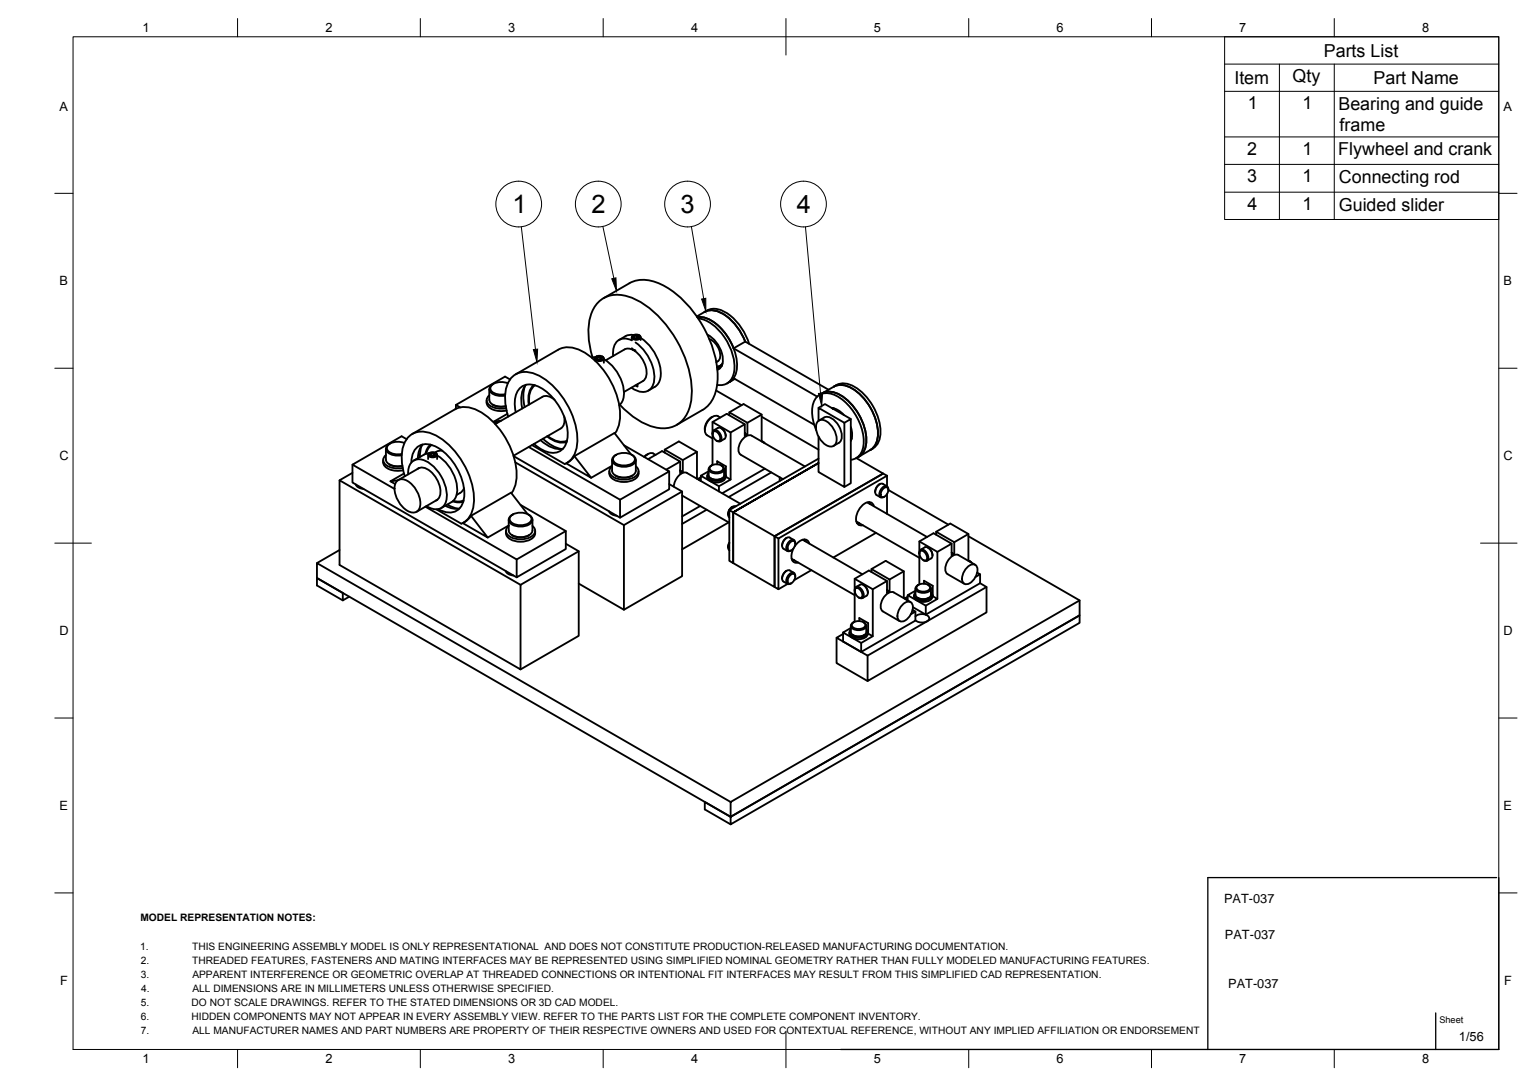
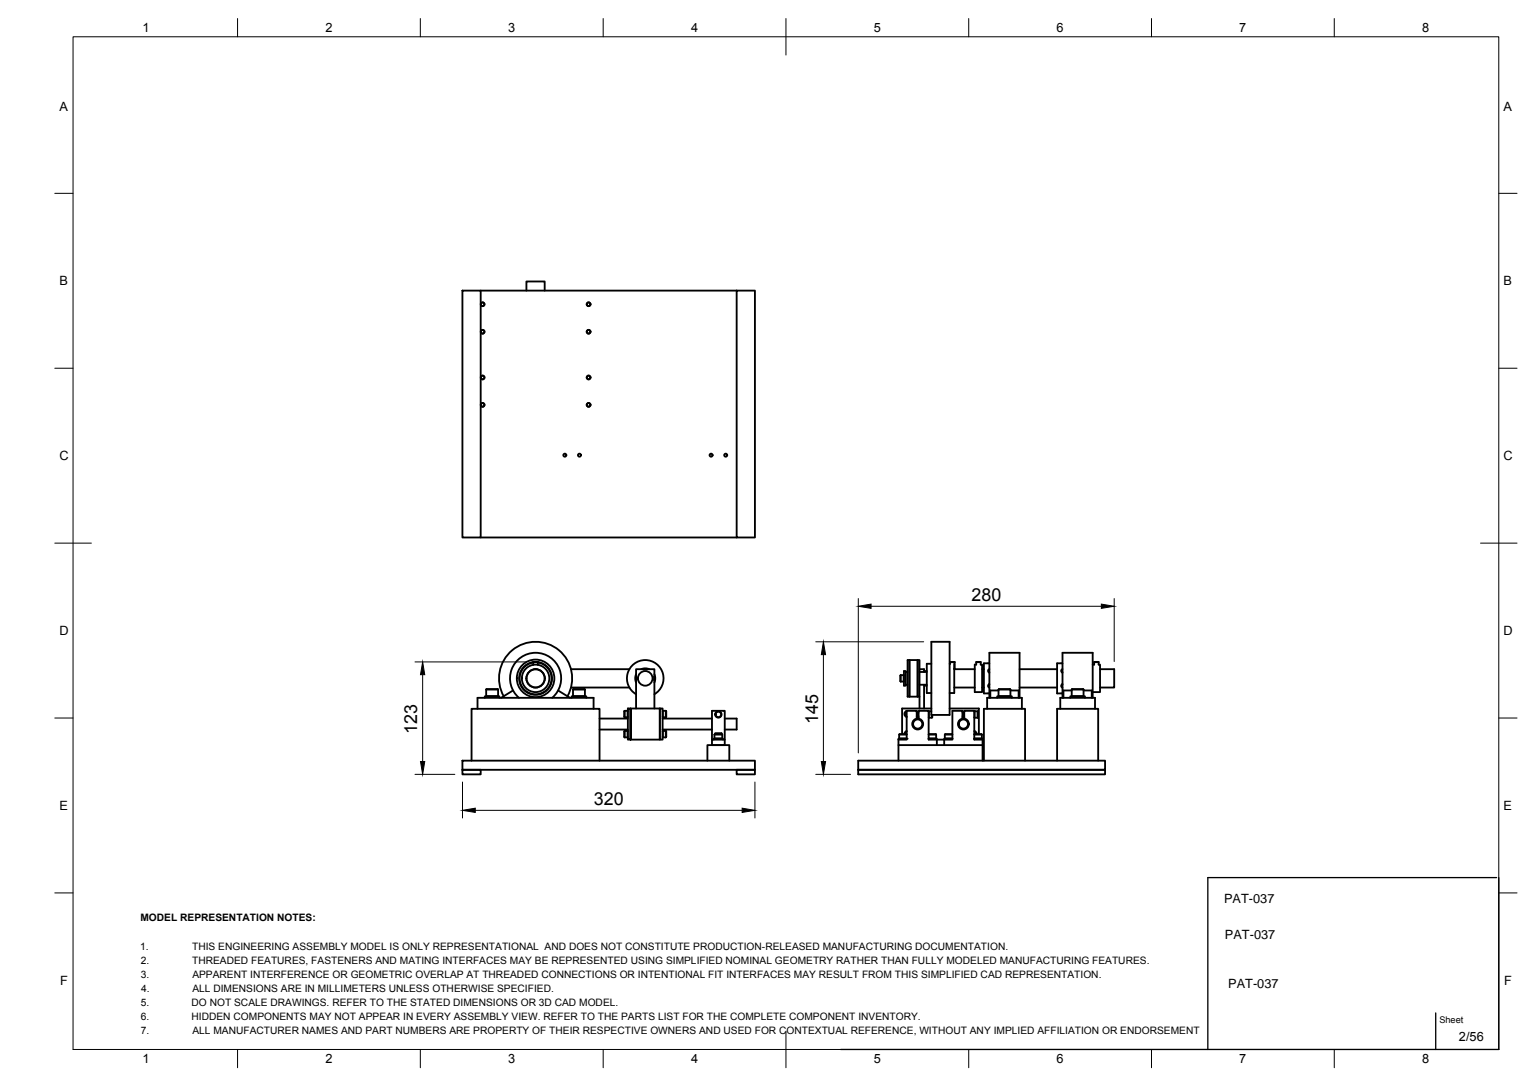
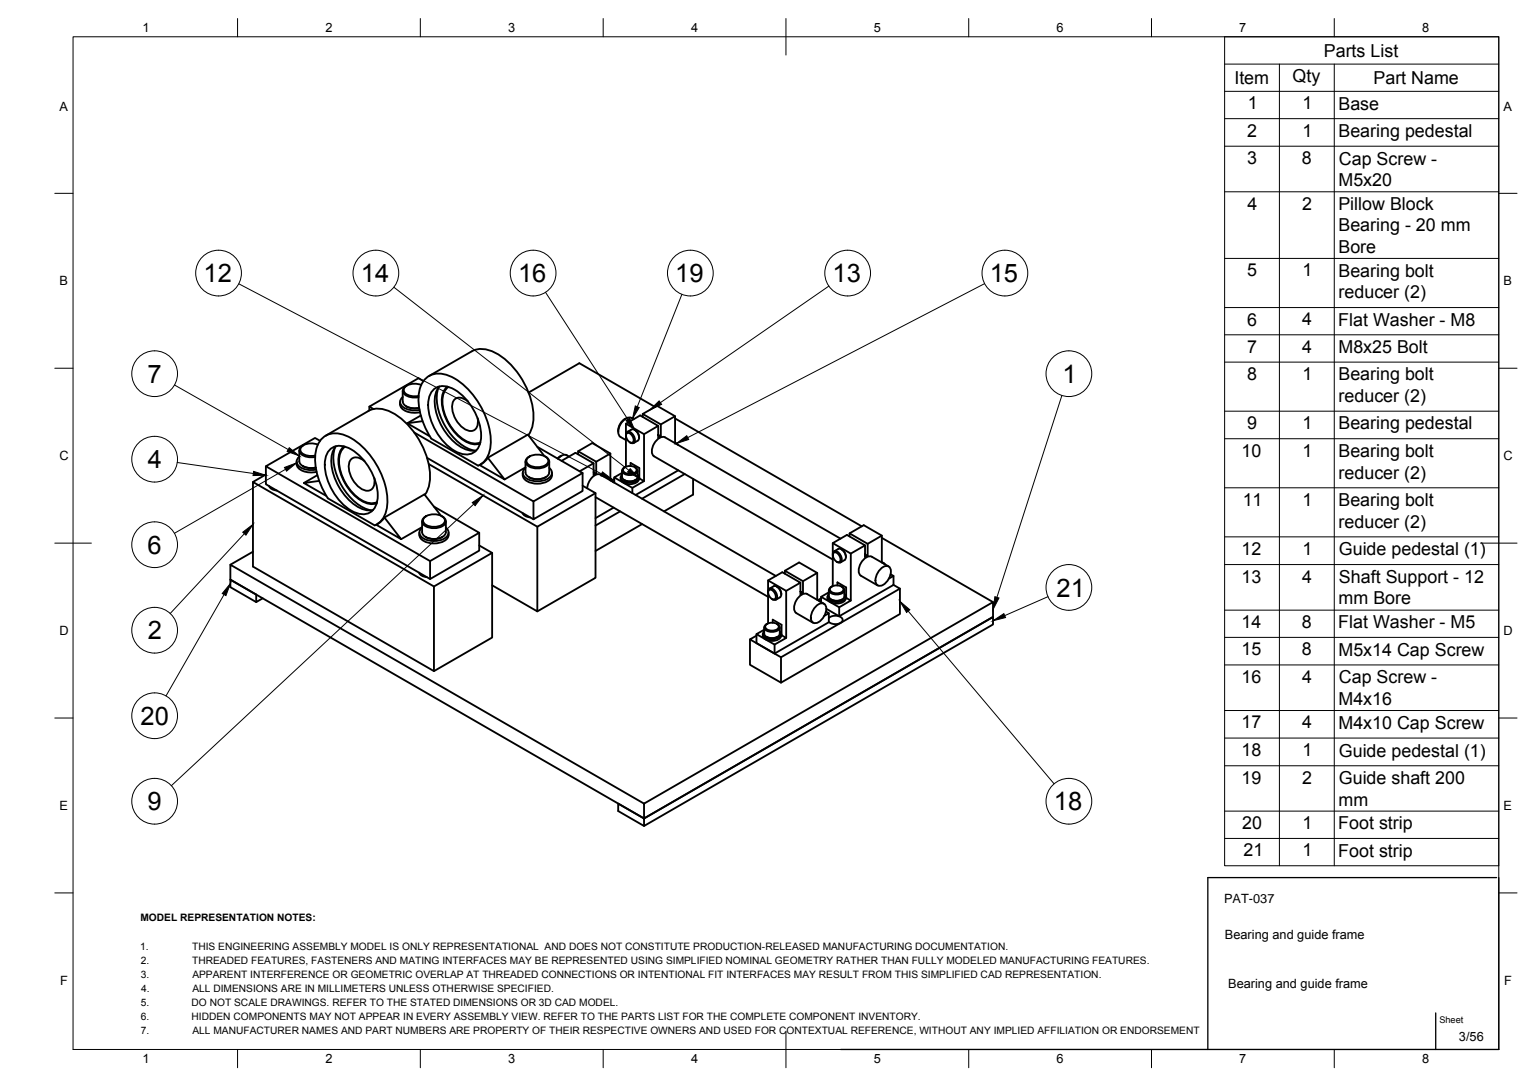
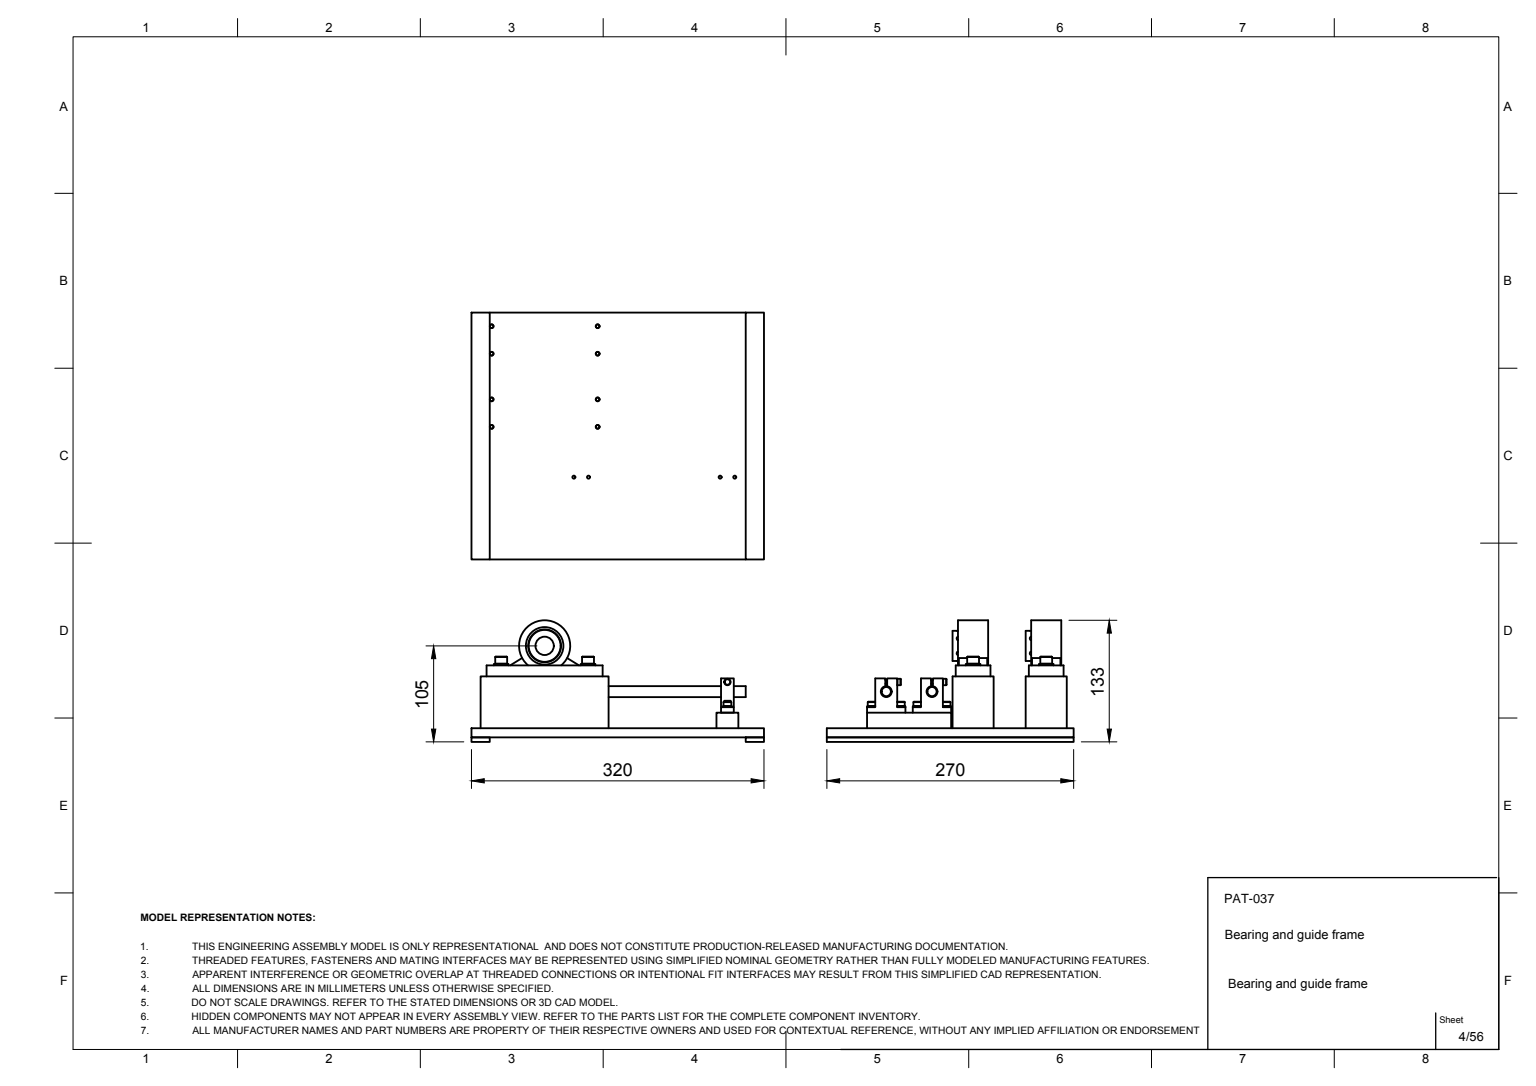
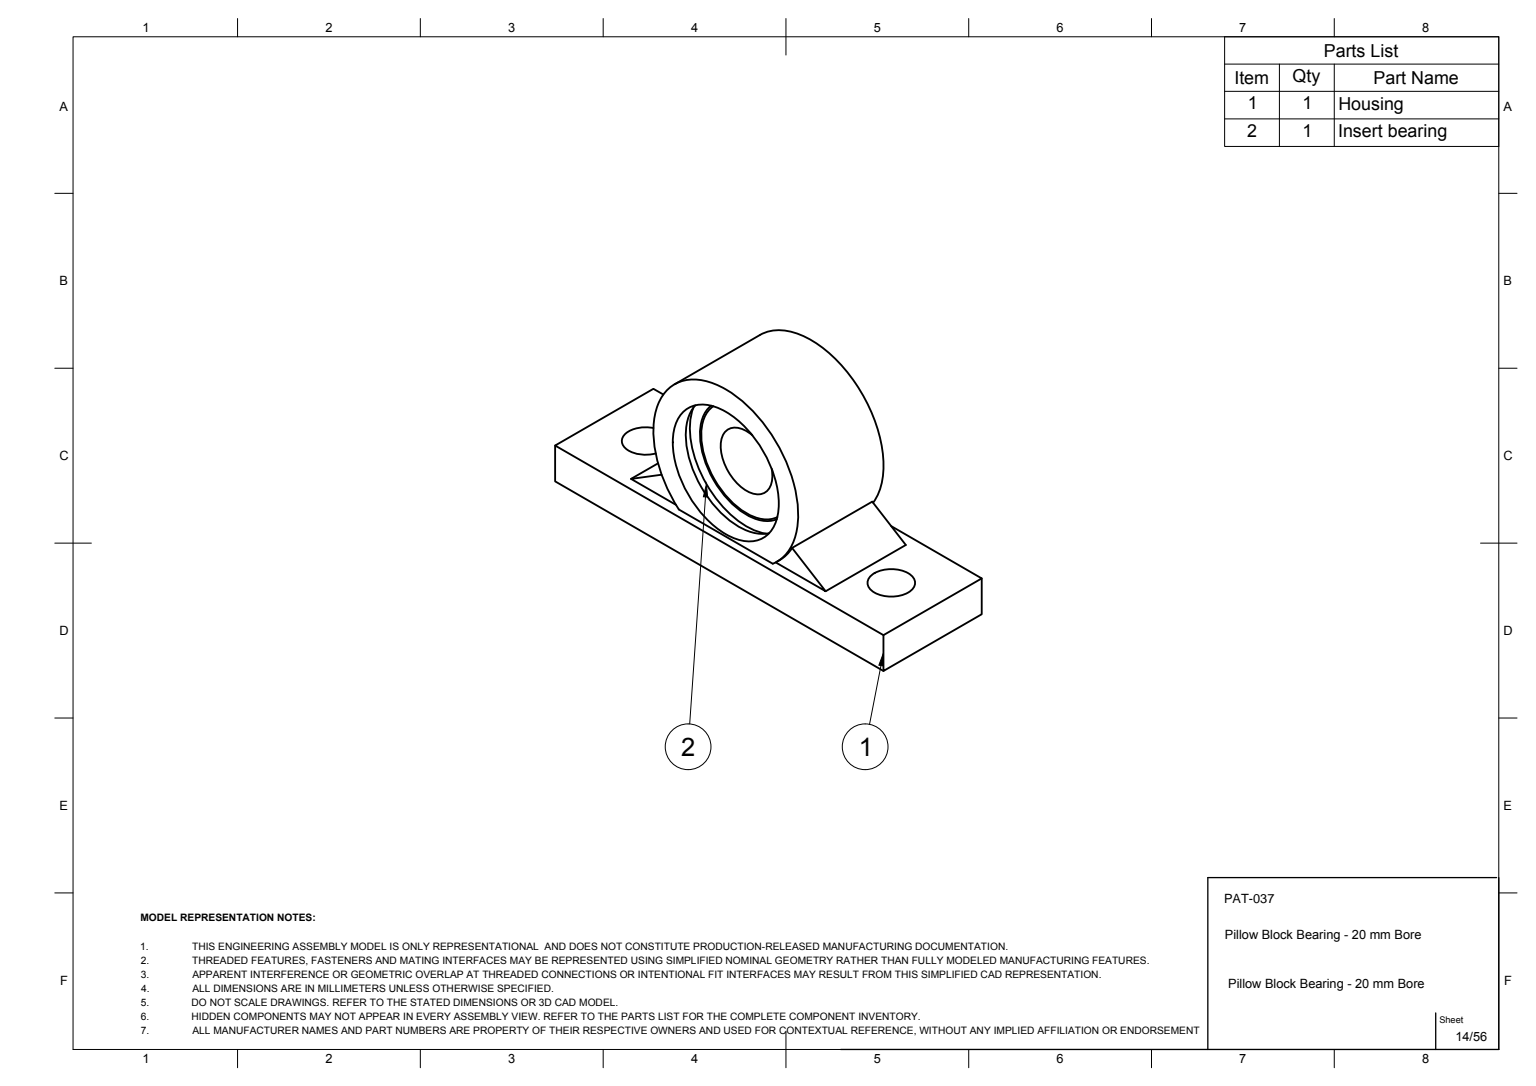
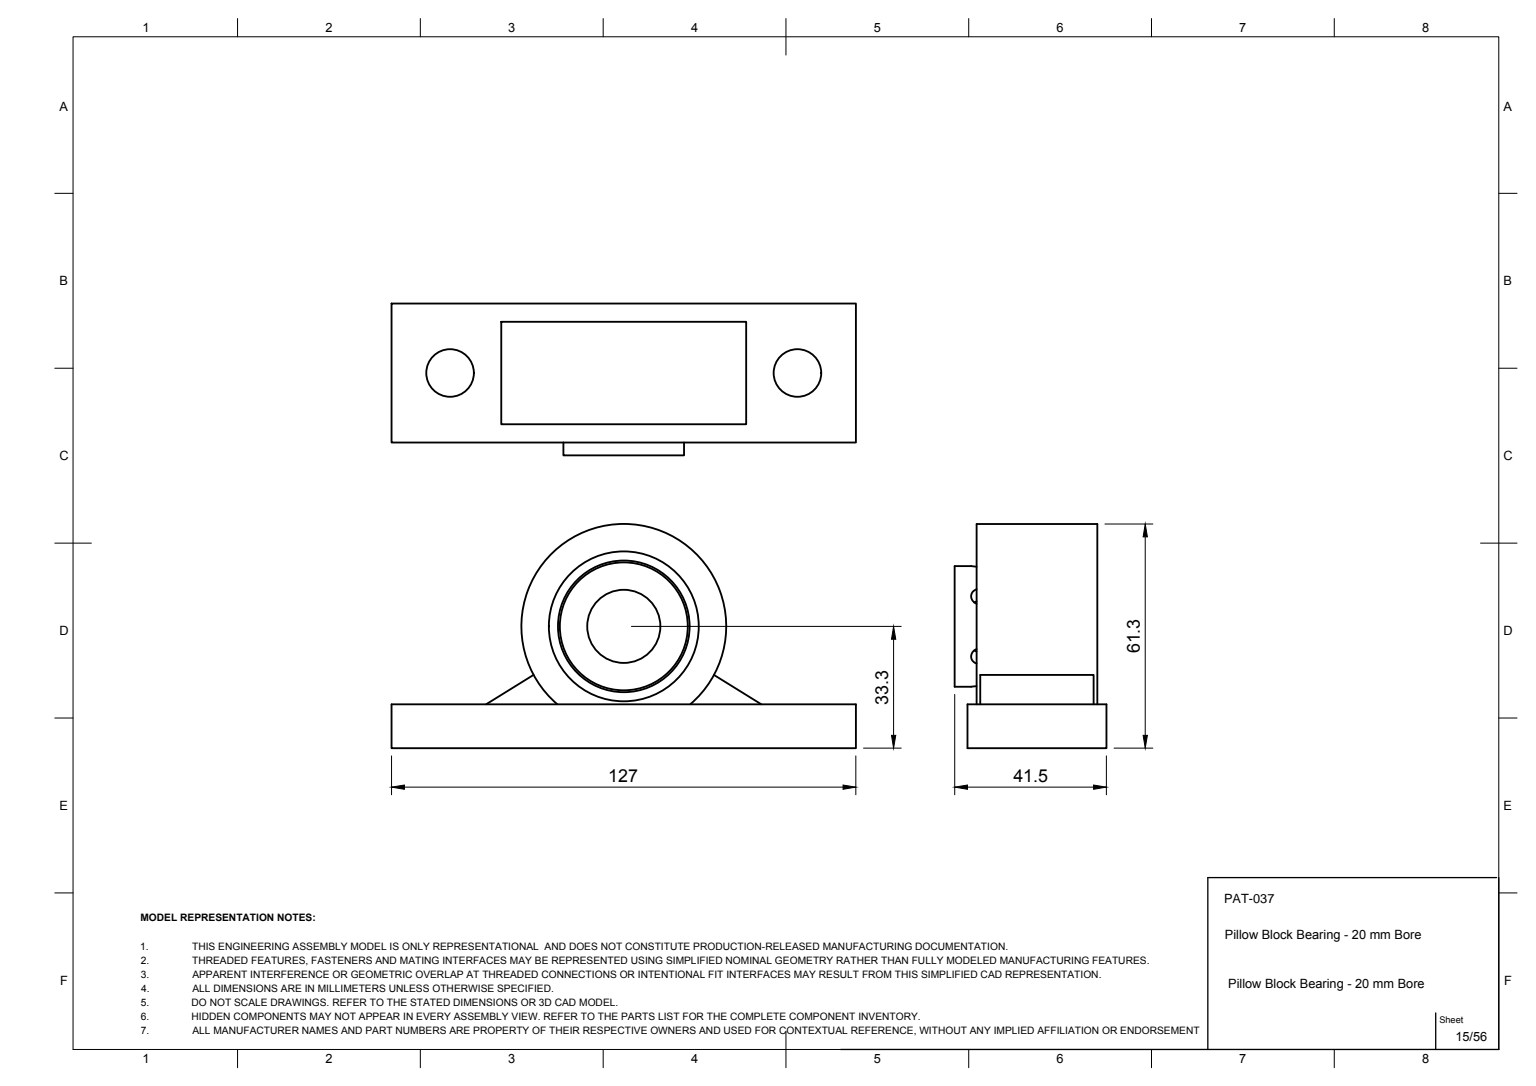
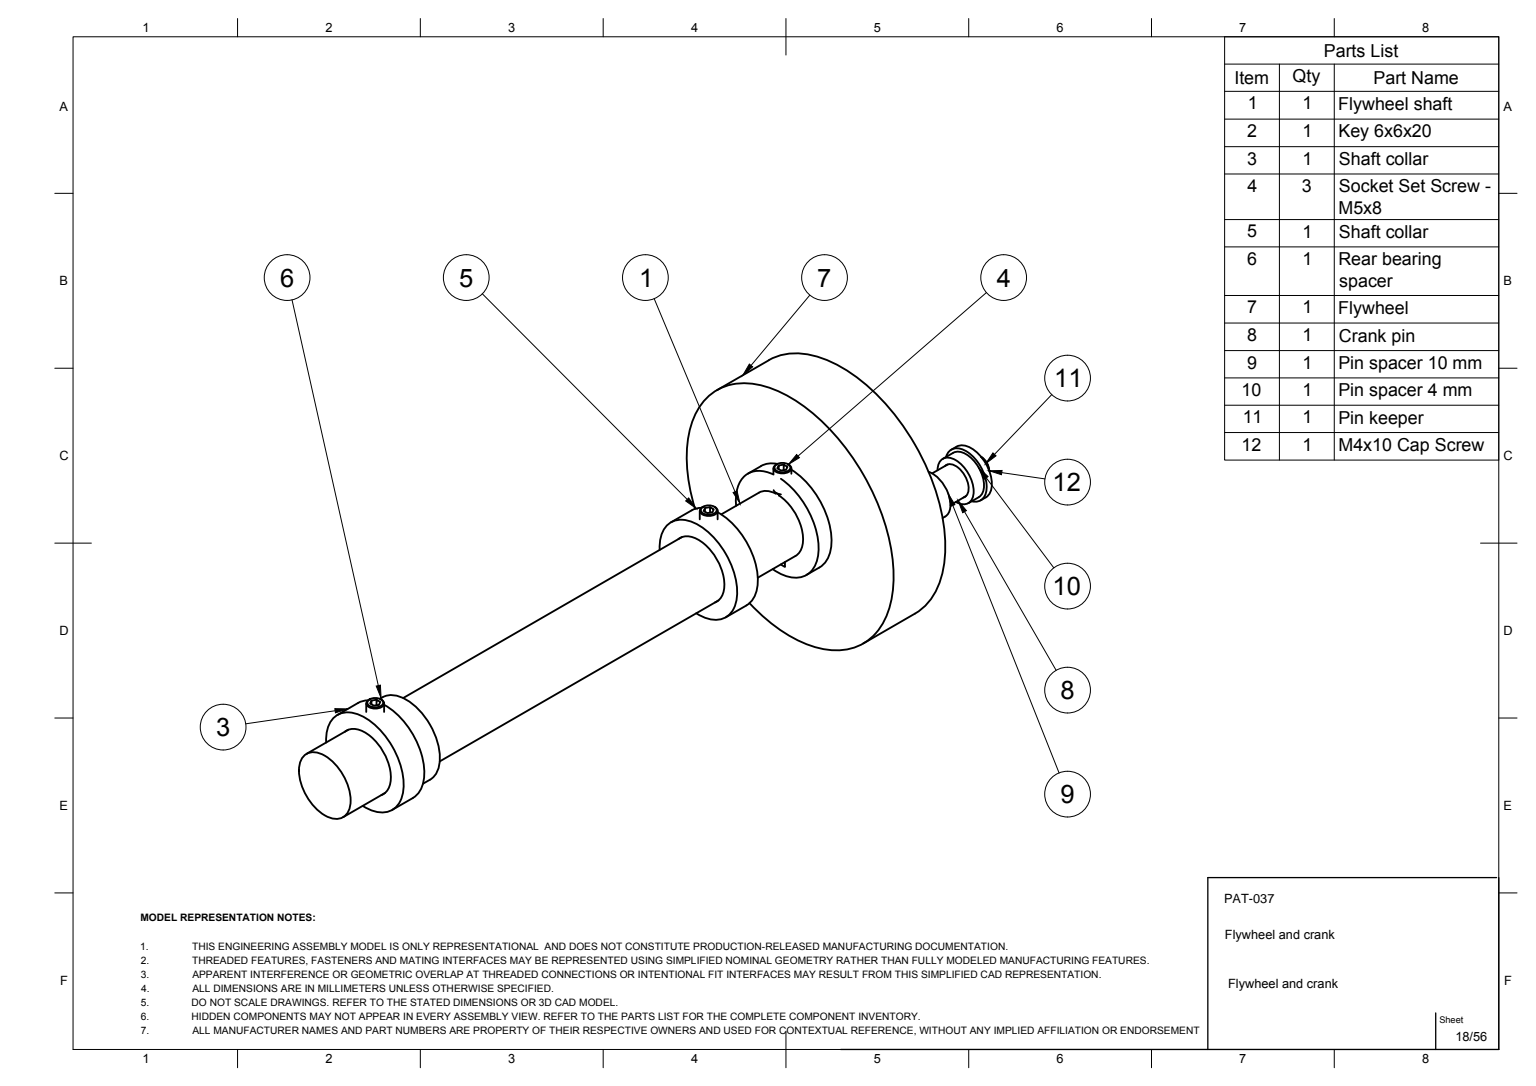
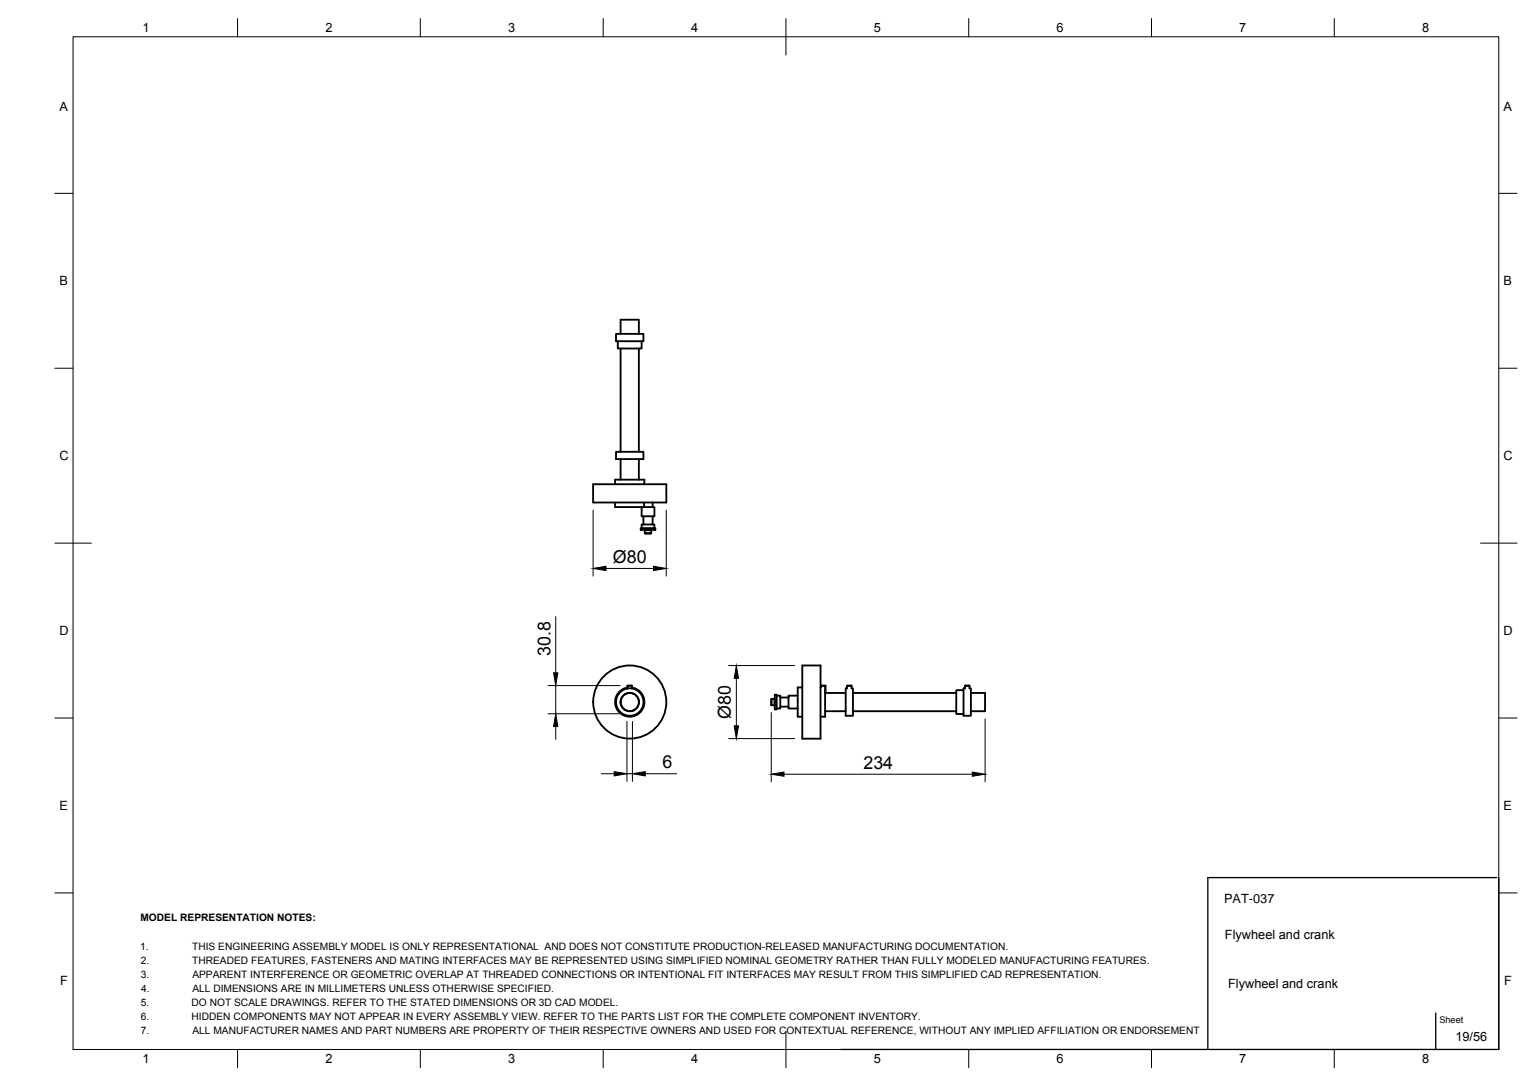
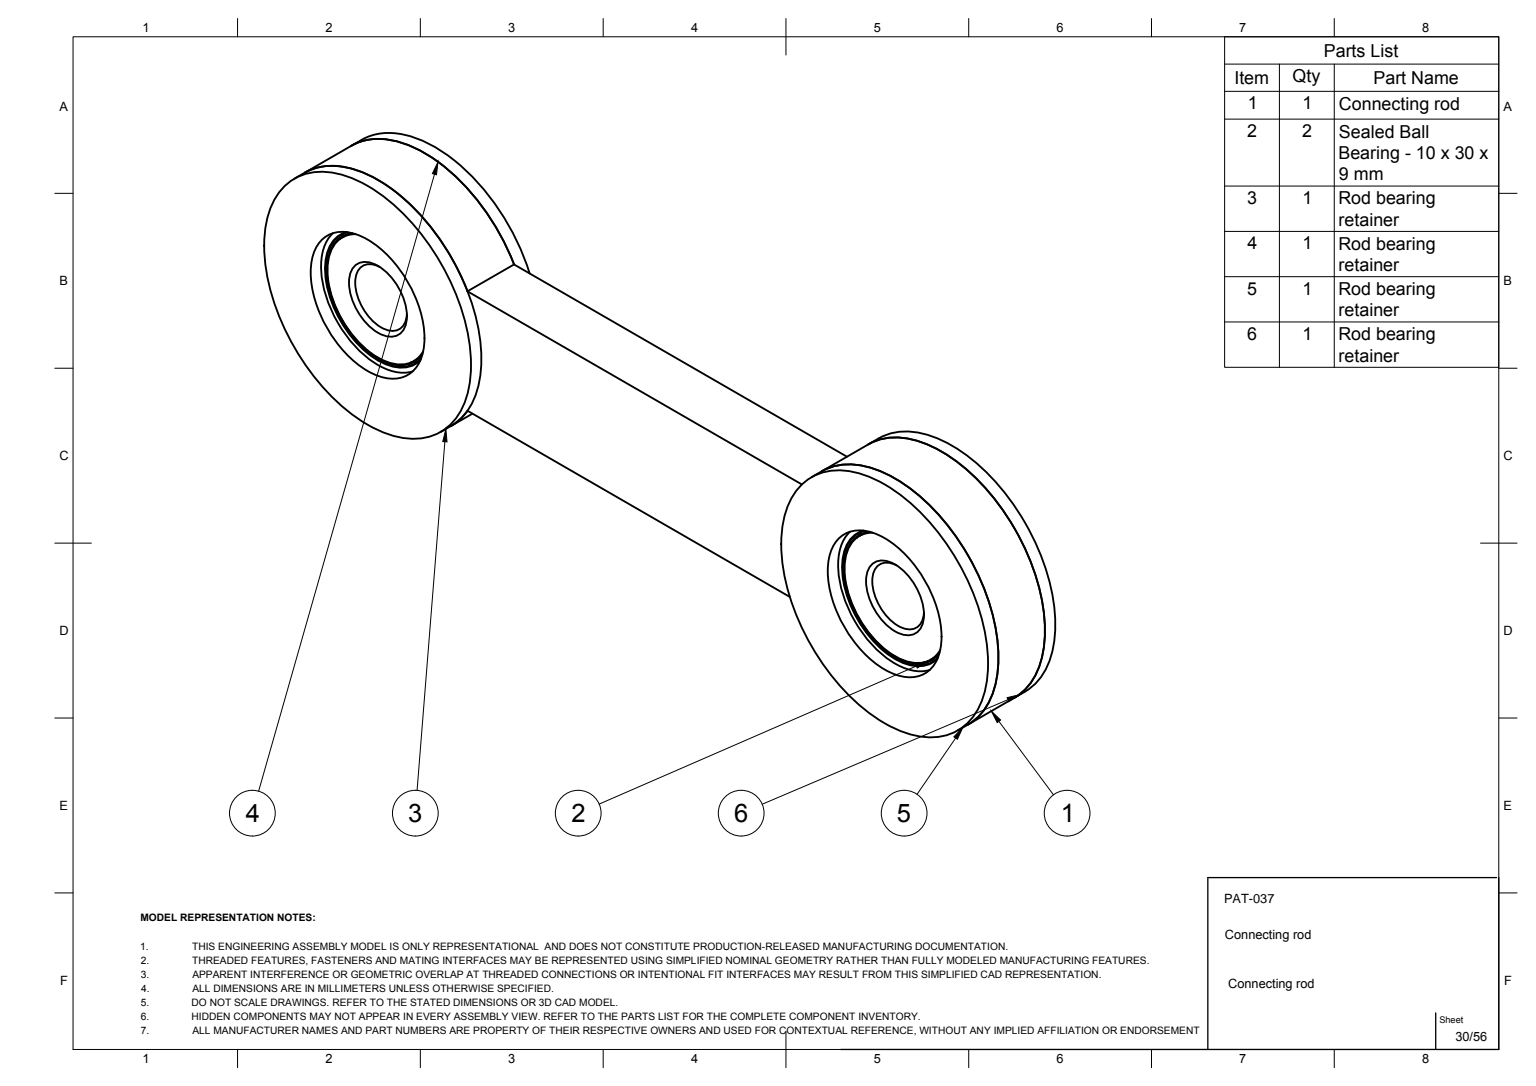
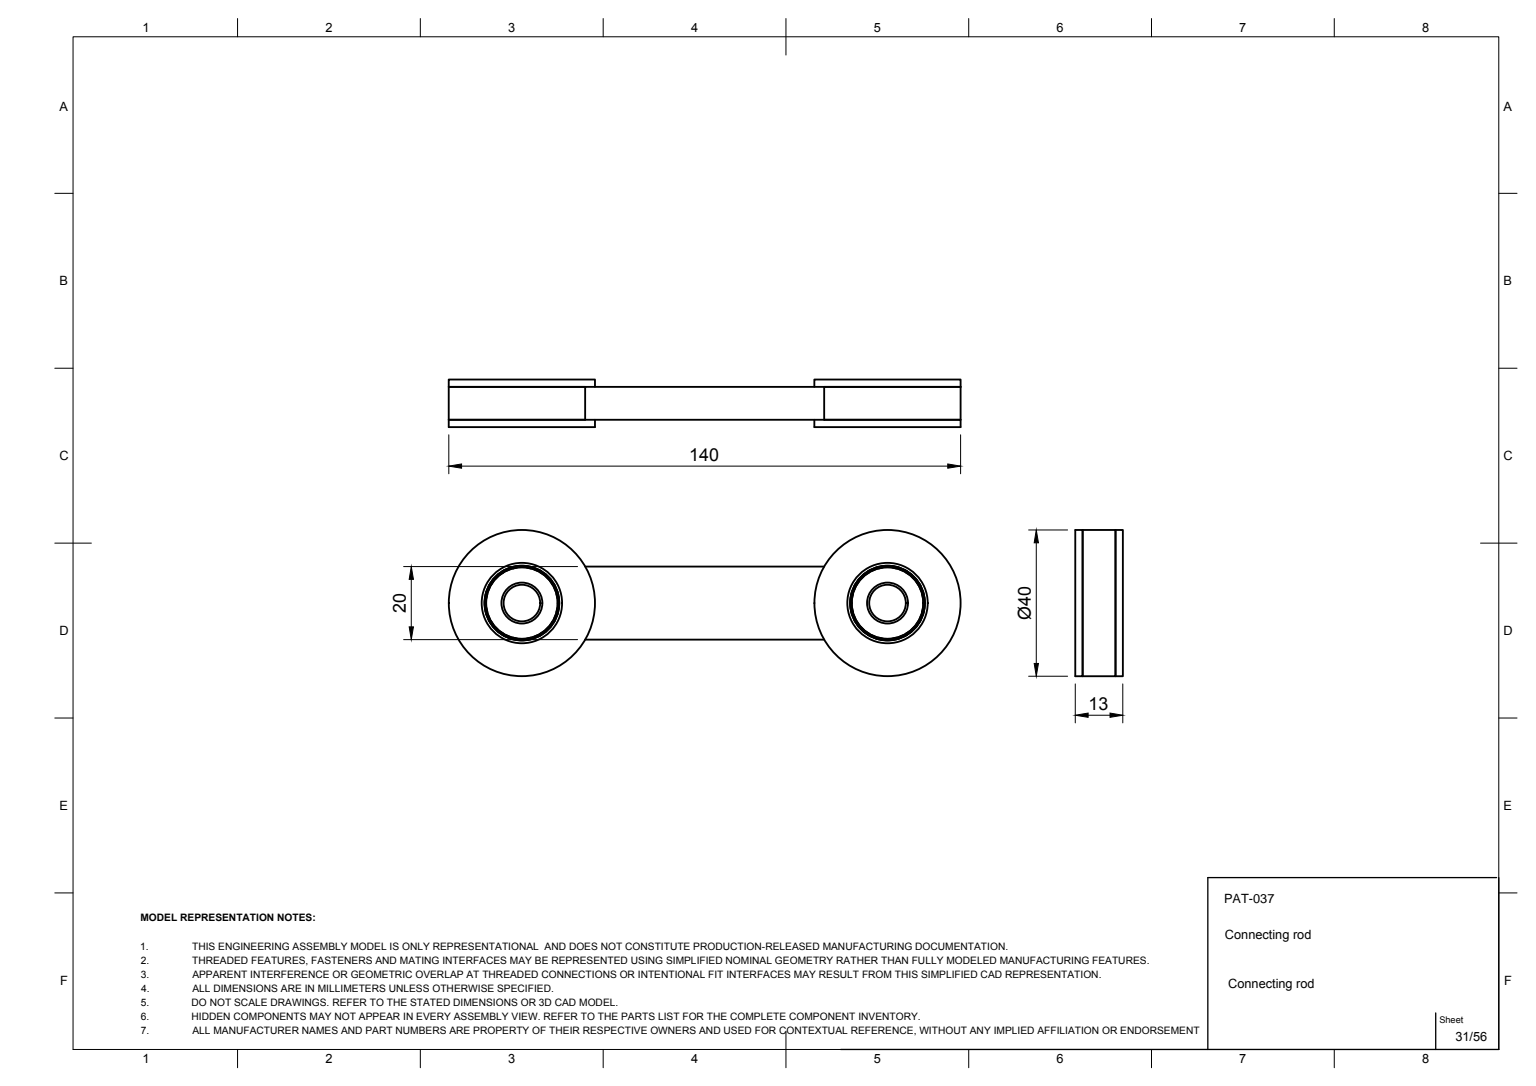
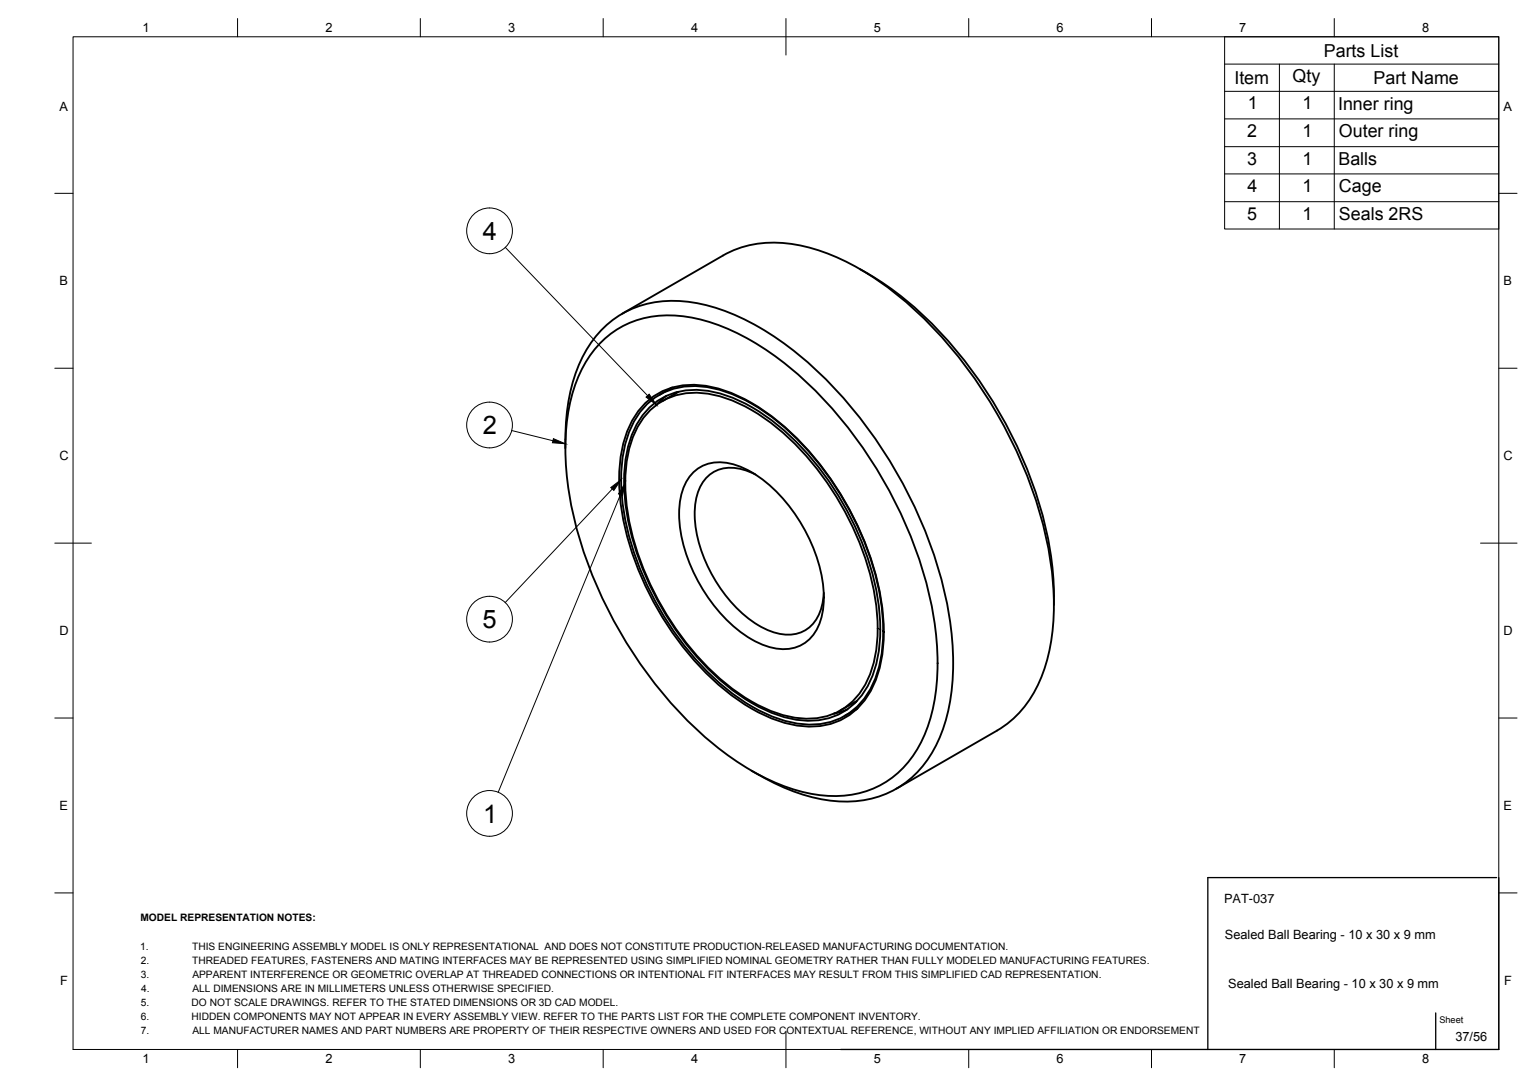
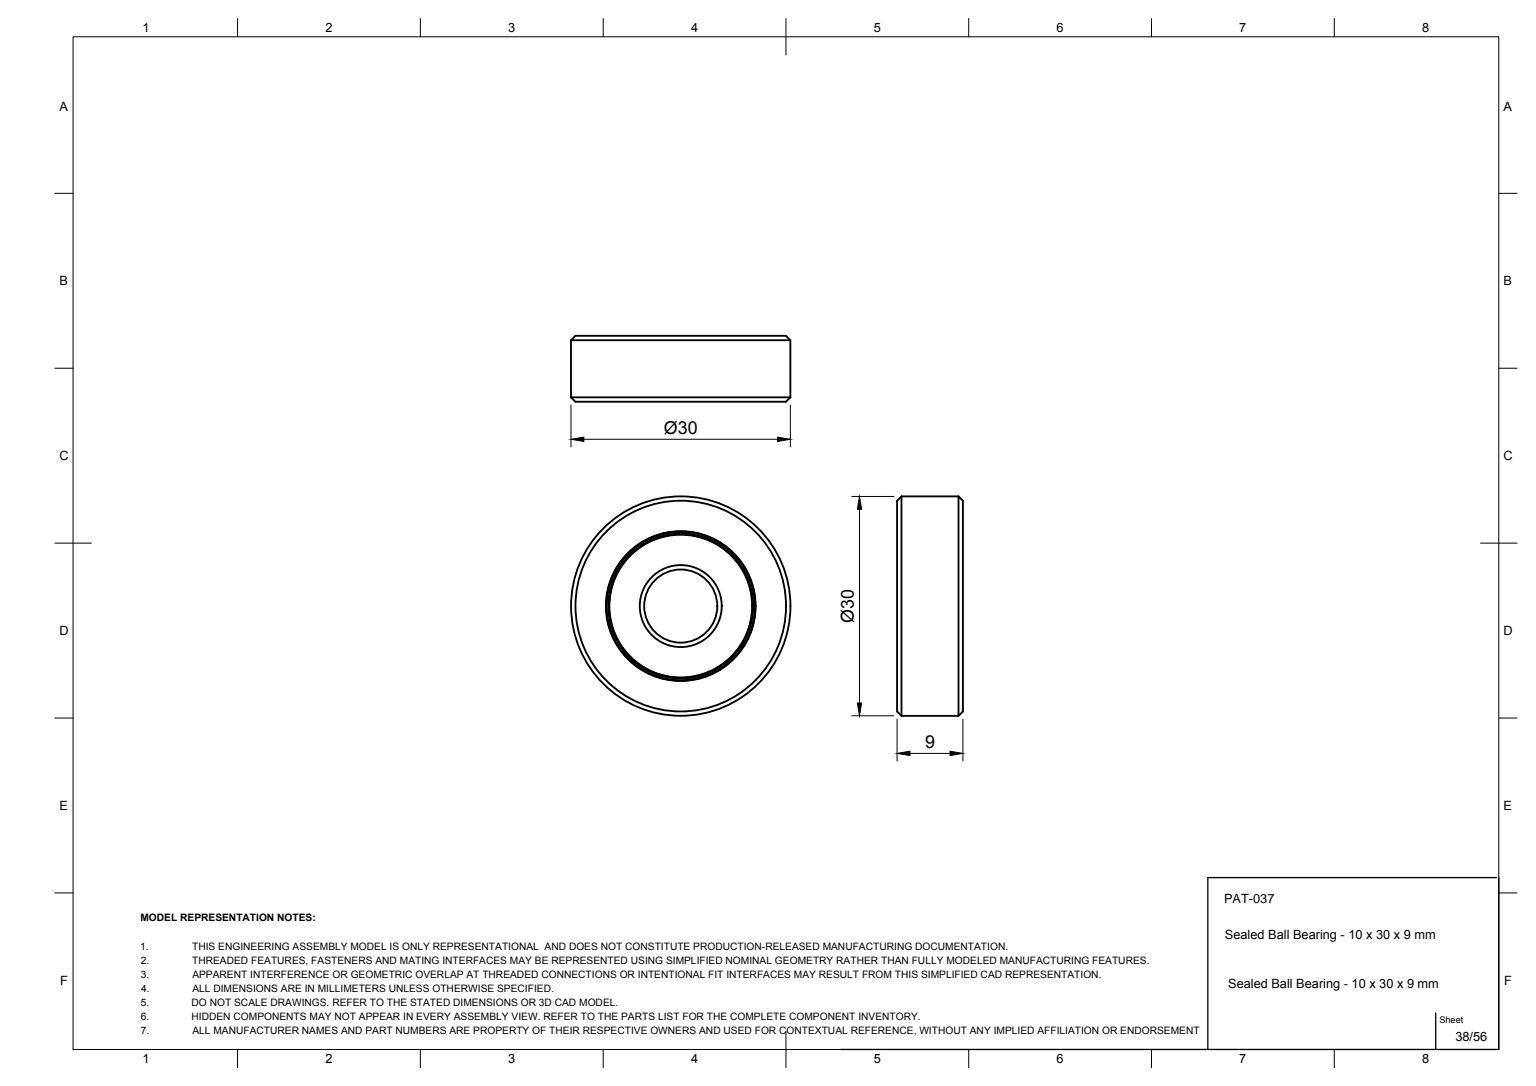
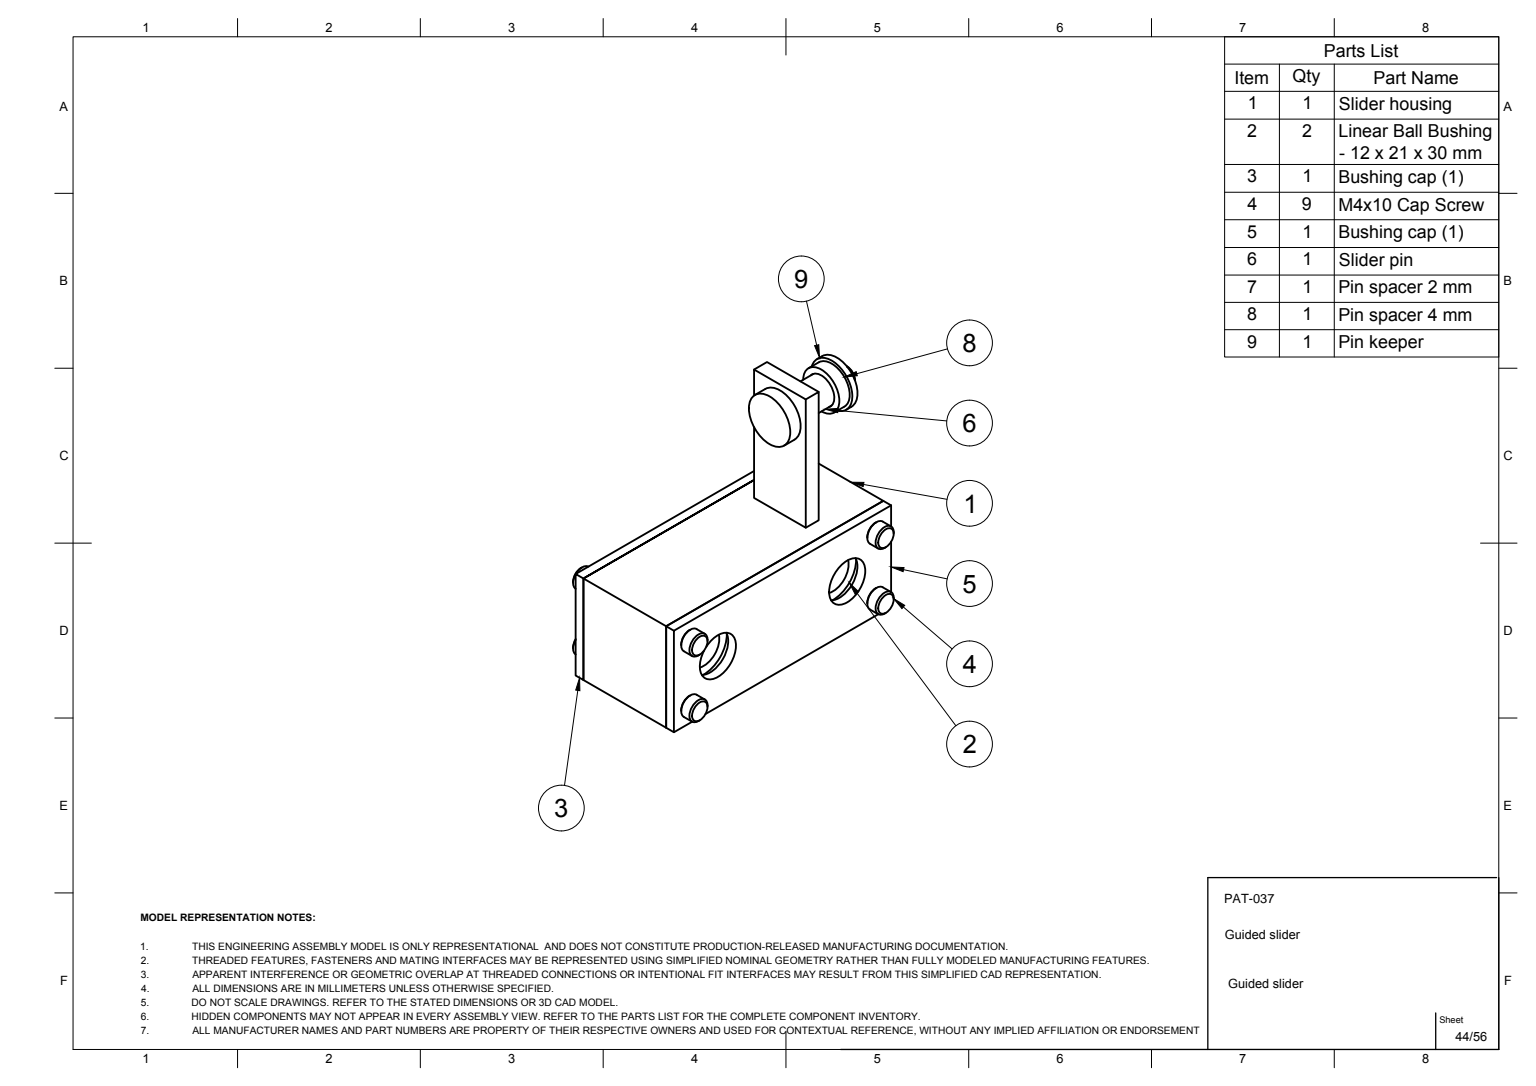
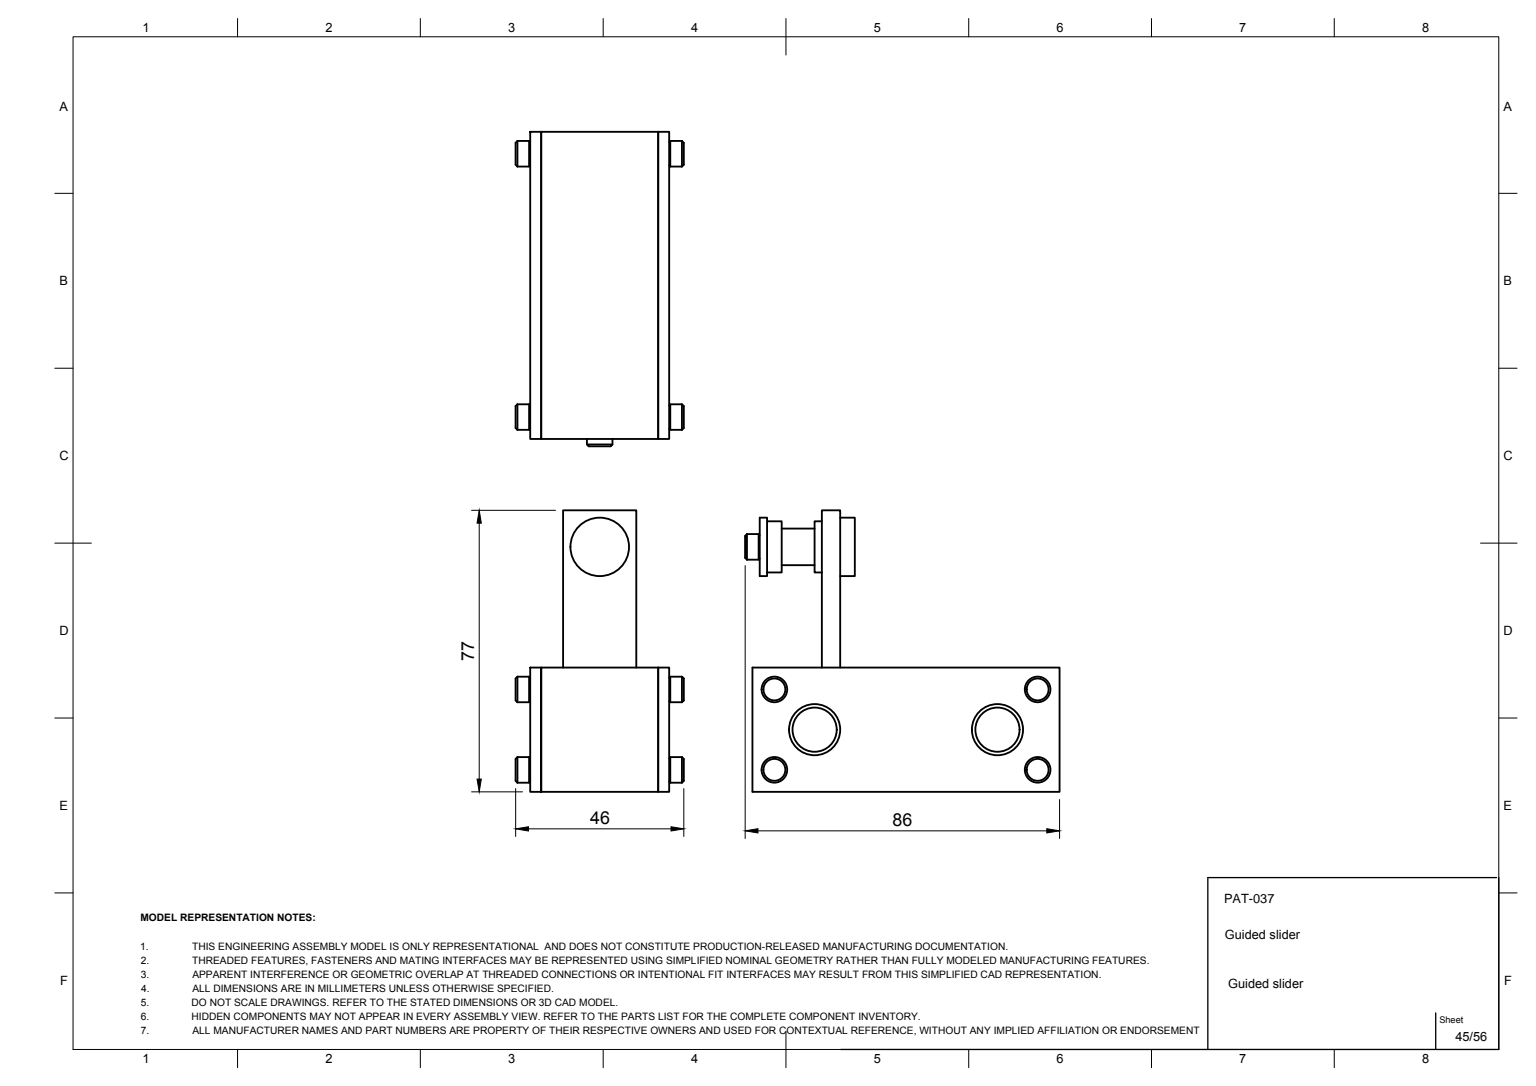
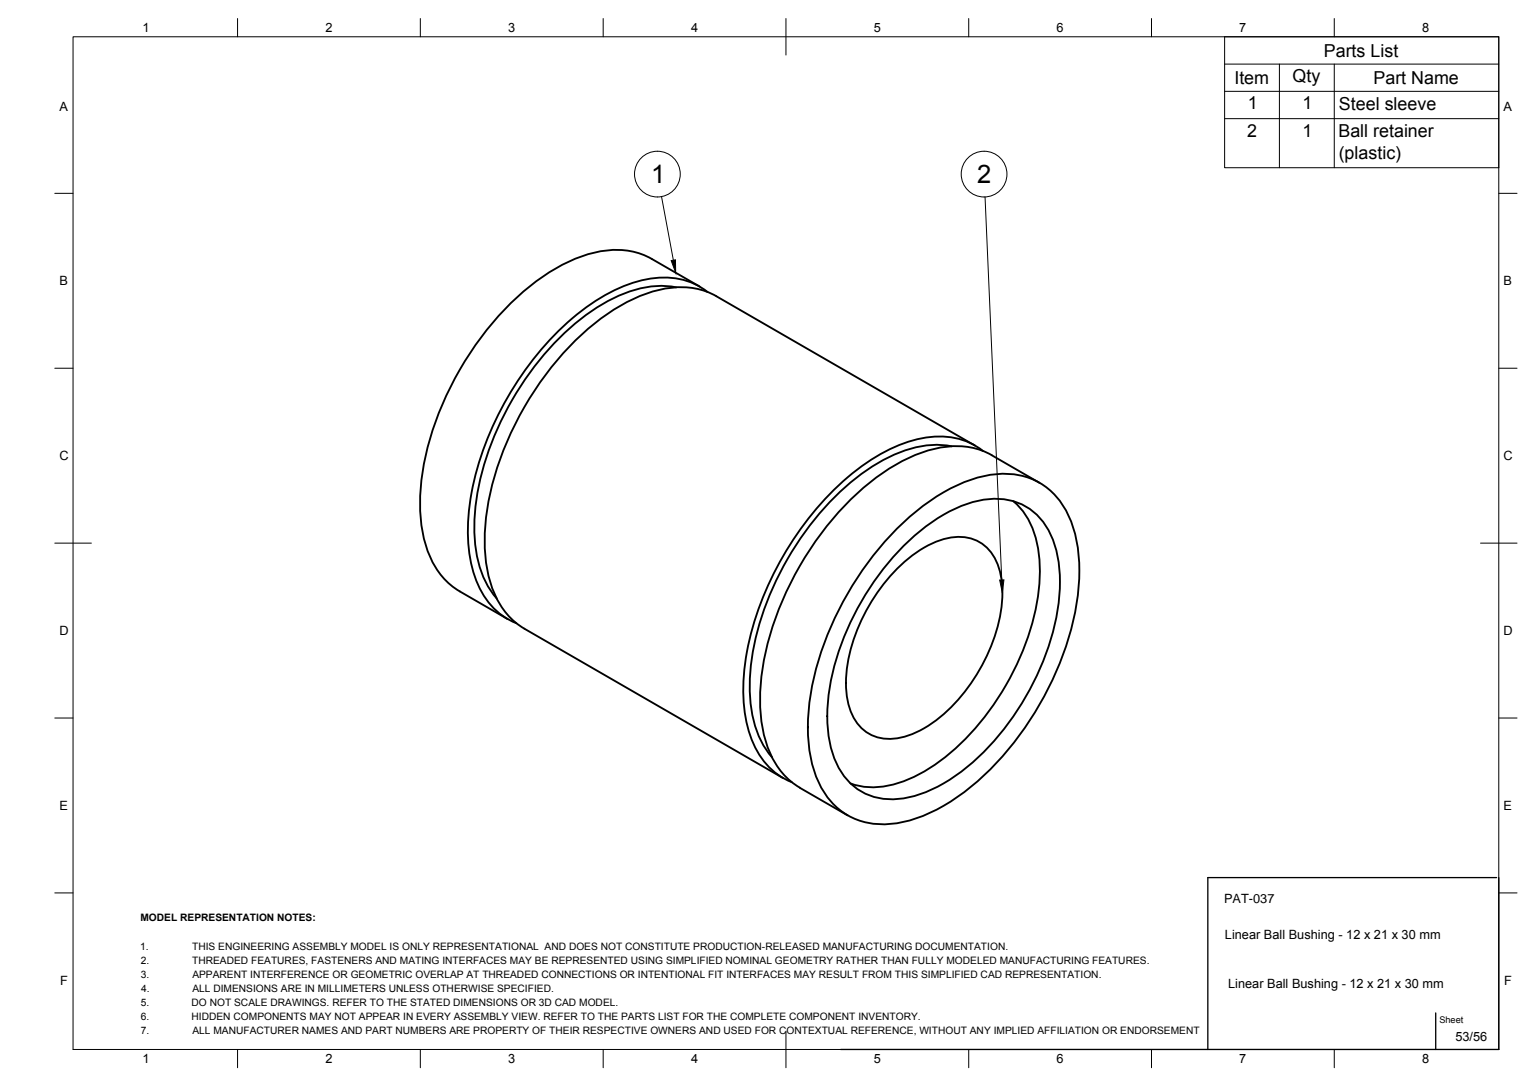
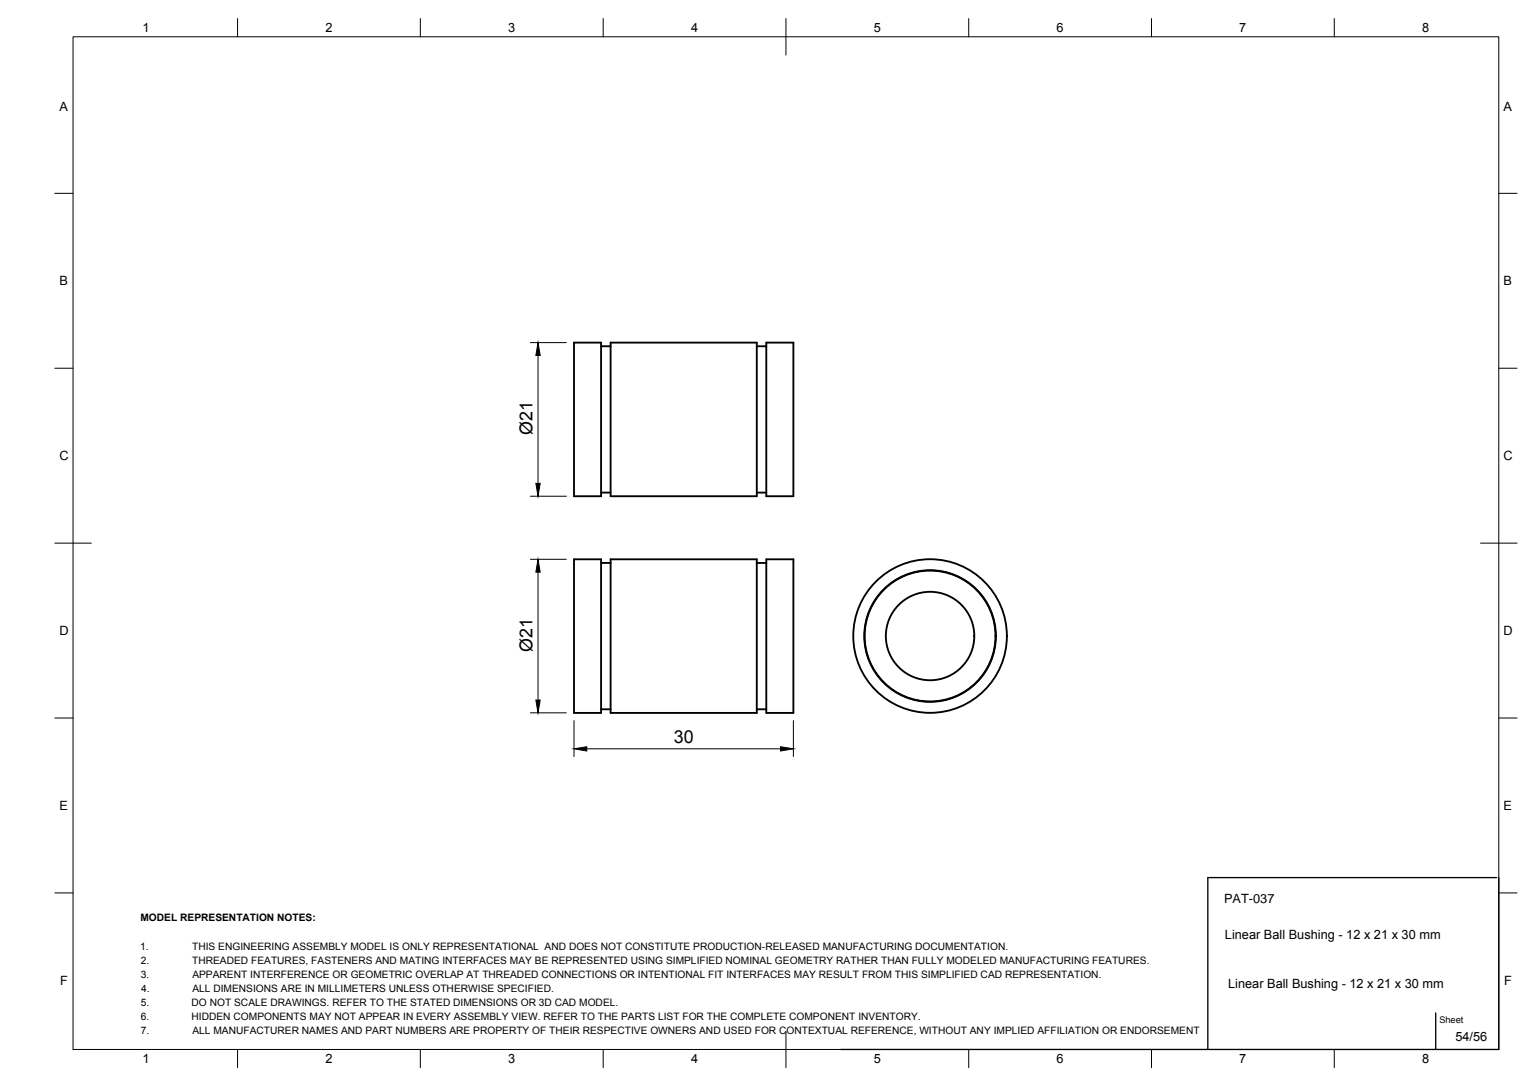
ISO-10303-21;
HEADER;
/* Generated by software containing ST-Developer
 * from STEP Tools, Inc. (www.steptools.com) 
 */

FILE_DESCRIPTION(
/* description */ ('Flywheel Crank-Slider'),
/* implementation_level */ '2;1');

FILE_NAME(
/* name */ 'PAT-037',
/* time_stamp */ '2026-10-28T03:23:13-07:00',
/* author */ (''),
/* organization */ (''),
/* preprocessor_version */ 'ST-DEVELOPER v20.2',
/* originating_system */ 'Autodesk Translation Framework v15.17.0.0',
/* authorisation */ '');

FILE_SCHEMA (('AUTOMOTIVE_DESIGN { 1 0 10303 214 3 1 1 }'));
ENDSEC;

DATA;
#10=MECHANICAL_DESIGN_GEOMETRIC_PRESENTATION_REPRESENTATION('',(#668,#669,
#670,#671,#672,#673,#674,#675,#676,#677,#678,#679,#680,#681,#682,#683,#684,
#685,#686,#687,#688,#689,#690,#691,#692,#693,#694,#695,#696,#697,#698,#699,
#700,#701,#702,#703,#704,#705,#706,#707,#708,#709,#710,#711,#712,#713,#714,
#715,#716,#717,#718,#719,#720,#721,#722,#723,#724,#725,#726,#727,#728),
#17322);
#11=TOROIDAL_SURFACE('',#10395,1.,0.247676);
#12=TOROIDAL_SURFACE('',#10415,1.,0.247676);
#13=ITEM_DEFINED_TRANSFORMATION($,$,#9973,#10042);
#14=ITEM_DEFINED_TRANSFORMATION($,$,#10014,#10043);
#15=ITEM_DEFINED_TRANSFORMATION($,$,#10394,#10522);
#16=ITEM_DEFINED_TRANSFORMATION($,$,#10414,#10523);
#17=ITEM_DEFINED_TRANSFORMATION($,$,#10434,#10524);
#18=ITEM_DEFINED_TRANSFORMATION($,$,#10451,#10525);
#19=ITEM_DEFINED_TRANSFORMATION($,$,#10505,#10526);
#20=ITEM_DEFINED_TRANSFORMATION($,$,#10340,#10527);
#21=ITEM_DEFINED_TRANSFORMATION($,$,#10357,#10528);
#22=ITEM_DEFINED_TRANSFORMATION($,$,#10366,#10529);
#23=ITEM_DEFINED_TRANSFORMATION($,$,#10375,#10530);
#24=ITEM_DEFINED_TRANSFORMATION($,$,#10384,#10531);
#25=ITEM_DEFINED_TRANSFORMATION($,$,#10393,#10532);
#26=ITEM_DEFINED_TRANSFORMATION($,$,#10393,#10533);
#27=ITEM_DEFINED_TRANSFORMATION($,$,#10660,#10709);
#28=ITEM_DEFINED_TRANSFORMATION($,$,#10692,#10710);
#29=ITEM_DEFINED_TRANSFORMATION($,$,#9687,#10735);
#30=ITEM_DEFINED_TRANSFORMATION($,$,#9730,#10736);
#31=ITEM_DEFINED_TRANSFORMATION($,$,#9773,#10737);
#32=ITEM_DEFINED_TRANSFORMATION($,$,#9782,#10738);
#33=ITEM_DEFINED_TRANSFORMATION($,$,#9791,#10739);
#34=ITEM_DEFINED_TRANSFORMATION($,$,#9834,#10740);
#35=ITEM_DEFINED_TRANSFORMATION($,$,#9843,#10741);
#36=ITEM_DEFINED_TRANSFORMATION($,$,#9852,#10742);
#37=ITEM_DEFINED_TRANSFORMATION($,$,#9892,#10743);
#38=ITEM_DEFINED_TRANSFORMATION($,$,#9932,#10744);
#39=ITEM_DEFINED_TRANSFORMATION($,$,#9939,#10745);
#40=ITEM_DEFINED_TRANSFORMATION($,$,#9946,#10746);
#41=ITEM_DEFINED_TRANSFORMATION($,$,#9946,#10747);
#42=ITEM_DEFINED_TRANSFORMATION($,$,#9946,#10748);
#43=ITEM_DEFINED_TRANSFORMATION($,$,#9946,#10749);
#44=ITEM_DEFINED_TRANSFORMATION($,$,#9972,#10750);
#45=ITEM_DEFINED_TRANSFORMATION($,$,#10044,#10751);
#46=ITEM_DEFINED_TRANSFORMATION($,$,#10053,#10752);
#47=ITEM_DEFINED_TRANSFORMATION($,$,#10044,#10753);
#48=ITEM_DEFINED_TRANSFORMATION($,$,#10053,#10754);
#49=ITEM_DEFINED_TRANSFORMATION($,$,#9946,#10755);
#50=ITEM_DEFINED_TRANSFORMATION($,$,#9946,#10756);
#51=ITEM_DEFINED_TRANSFORMATION($,$,#9946,#10757);
#52=ITEM_DEFINED_TRANSFORMATION($,$,#9946,#10758);
#53=ITEM_DEFINED_TRANSFORMATION($,$,#9972,#10759);
#54=ITEM_DEFINED_TRANSFORMATION($,$,#10044,#10760);
#55=ITEM_DEFINED_TRANSFORMATION($,$,#10053,#10761);
#56=ITEM_DEFINED_TRANSFORMATION($,$,#10044,#10762);
#57=ITEM_DEFINED_TRANSFORMATION($,$,#10053,#10763);
#58=ITEM_DEFINED_TRANSFORMATION($,$,#10077,#10764);
#59=ITEM_DEFINED_TRANSFORMATION($,$,#10115,#10765);
#60=ITEM_DEFINED_TRANSFORMATION($,$,#10126,#10766);
#61=ITEM_DEFINED_TRANSFORMATION($,$,#10115,#10767);
#62=ITEM_DEFINED_TRANSFORMATION($,$,#10126,#10768);
#63=ITEM_DEFINED_TRANSFORMATION($,$,#10150,#10769);
#64=ITEM_DEFINED_TRANSFORMATION($,$,#10077,#10770);
#65=ITEM_DEFINED_TRANSFORMATION($,$,#10115,#10771);
#66=ITEM_DEFINED_TRANSFORMATION($,$,#10126,#10772);
#67=ITEM_DEFINED_TRANSFORMATION($,$,#10115,#10773);
#68=ITEM_DEFINED_TRANSFORMATION($,$,#10126,#10774);
#69=ITEM_DEFINED_TRANSFORMATION($,$,#10150,#10775);
#70=ITEM_DEFINED_TRANSFORMATION($,$,#10711,#10776);
#71=ITEM_DEFINED_TRANSFORMATION($,$,#10711,#10777);
#72=ITEM_DEFINED_TRANSFORMATION($,$,#10077,#10778);
#73=ITEM_DEFINED_TRANSFORMATION($,$,#10115,#10779);
#74=ITEM_DEFINED_TRANSFORMATION($,$,#10126,#10780);
#75=ITEM_DEFINED_TRANSFORMATION($,$,#10115,#10781);
#76=ITEM_DEFINED_TRANSFORMATION($,$,#10126,#10782);
#77=ITEM_DEFINED_TRANSFORMATION($,$,#10150,#10783);
#78=ITEM_DEFINED_TRANSFORMATION($,$,#10077,#10784);
#79=ITEM_DEFINED_TRANSFORMATION($,$,#10115,#10785);
#80=ITEM_DEFINED_TRANSFORMATION($,$,#10126,#10786);
#81=ITEM_DEFINED_TRANSFORMATION($,$,#10115,#10787);
#82=ITEM_DEFINED_TRANSFORMATION($,$,#10126,#10788);
#83=ITEM_DEFINED_TRANSFORMATION($,$,#10150,#10789);
#84=ITEM_DEFINED_TRANSFORMATION($,$,#10711,#10790);
#85=ITEM_DEFINED_TRANSFORMATION($,$,#10711,#10791);
#86=ITEM_DEFINED_TRANSFORMATION($,$,#10176,#10792);
#87=ITEM_DEFINED_TRANSFORMATION($,$,#10176,#10793);
#88=ITEM_DEFINED_TRANSFORMATION($,$,#10185,#10794);
#89=ITEM_DEFINED_TRANSFORMATION($,$,#10197,#10795);
#90=ITEM_DEFINED_TRANSFORMATION($,$,#10212,#10796);
#91=ITEM_DEFINED_TRANSFORMATION($,$,#10227,#10797);
#92=ITEM_DEFINED_TRANSFORMATION($,$,#10236,#10798);
#93=ITEM_DEFINED_TRANSFORMATION($,$,#10270,#10799);
#94=ITEM_DEFINED_TRANSFORMATION($,$,#10284,#10800);
#95=ITEM_DEFINED_TRANSFORMATION($,$,#10293,#10801);
#96=ITEM_DEFINED_TRANSFORMATION($,$,#10302,#10802);
#97=ITEM_DEFINED_TRANSFORMATION($,$,#10311,#10803);
#98=ITEM_DEFINED_TRANSFORMATION($,$,#10322,#10804);
#99=ITEM_DEFINED_TRANSFORMATION($,$,#10322,#10805);
#100=ITEM_DEFINED_TRANSFORMATION($,$,#10322,#10806);
#101=ITEM_DEFINED_TRANSFORMATION($,$,#10711,#10807);
#102=ITEM_DEFINED_TRANSFORMATION($,$,#10535,#10808);
#103=ITEM_DEFINED_TRANSFORMATION($,$,#10568,#10809);
#104=ITEM_DEFINED_TRANSFORMATION($,$,#10593,#10810);
#105=ITEM_DEFINED_TRANSFORMATION($,$,#10618,#10811);
#106=ITEM_DEFINED_TRANSFORMATION($,$,#10632,#10812);
#107=ITEM_DEFINED_TRANSFORMATION($,$,#10641,#10813);
#108=ITEM_DEFINED_TRANSFORMATION($,$,#10650,#10814);
#109=ITEM_DEFINED_TRANSFORMATION($,$,#10659,#10815);
#110=ITEM_DEFINED_TRANSFORMATION($,$,#10659,#10816);
#111=ITEM_DEFINED_TRANSFORMATION($,$,#10711,#10817);
#112=ITEM_DEFINED_TRANSFORMATION($,$,#10711,#10818);
#113=ITEM_DEFINED_TRANSFORMATION($,$,#10711,#10819);
#114=ITEM_DEFINED_TRANSFORMATION($,$,#10711,#10820);
#115=ITEM_DEFINED_TRANSFORMATION($,$,#10711,#10821);
#116=ITEM_DEFINED_TRANSFORMATION($,$,#10711,#10822);
#117=ITEM_DEFINED_TRANSFORMATION($,$,#10711,#10823);
#118=ITEM_DEFINED_TRANSFORMATION($,$,#10711,#10824);
#119=ITEM_DEFINED_TRANSFORMATION($,$,#10711,#10825);
#120=ITEM_DEFINED_TRANSFORMATION($,$,#9686,#10826);
#121=ITEM_DEFINED_TRANSFORMATION($,$,#10184,#10827);
#122=ITEM_DEFINED_TRANSFORMATION($,$,#10339,#10828);
#123=ITEM_DEFINED_TRANSFORMATION($,$,#10534,#10829);
#124=(
REPRESENTATION_RELATIONSHIP($,$,#17573,#17572)
REPRESENTATION_RELATIONSHIP_WITH_TRANSFORMATION(#13)
SHAPE_REPRESENTATION_RELATIONSHIP()
);
#125=(
REPRESENTATION_RELATIONSHIP($,$,#17574,#17572)
REPRESENTATION_RELATIONSHIP_WITH_TRANSFORMATION(#14)
SHAPE_REPRESENTATION_RELATIONSHIP()
);
#126=(
REPRESENTATION_RELATIONSHIP($,$,#17601,#17600)
REPRESENTATION_RELATIONSHIP_WITH_TRANSFORMATION(#15)
SHAPE_REPRESENTATION_RELATIONSHIP()
);
#127=(
REPRESENTATION_RELATIONSHIP($,$,#17602,#17600)
REPRESENTATION_RELATIONSHIP_WITH_TRANSFORMATION(#16)
SHAPE_REPRESENTATION_RELATIONSHIP()
);
#128=(
REPRESENTATION_RELATIONSHIP($,$,#17603,#17600)
REPRESENTATION_RELATIONSHIP_WITH_TRANSFORMATION(#17)
SHAPE_REPRESENTATION_RELATIONSHIP()
);
#129=(
REPRESENTATION_RELATIONSHIP($,$,#17604,#17600)
REPRESENTATION_RELATIONSHIP_WITH_TRANSFORMATION(#18)
SHAPE_REPRESENTATION_RELATIONSHIP()
);
#130=(
REPRESENTATION_RELATIONSHIP($,$,#17605,#17600)
REPRESENTATION_RELATIONSHIP_WITH_TRANSFORMATION(#19)
SHAPE_REPRESENTATION_RELATIONSHIP()
);
#131=(
REPRESENTATION_RELATIONSHIP($,$,#17595,#17594)
REPRESENTATION_RELATIONSHIP_WITH_TRANSFORMATION(#20)
SHAPE_REPRESENTATION_RELATIONSHIP()
);
#132=(
REPRESENTATION_RELATIONSHIP($,$,#17596,#17594)
REPRESENTATION_RELATIONSHIP_WITH_TRANSFORMATION(#21)
SHAPE_REPRESENTATION_RELATIONSHIP()
);
#133=(
REPRESENTATION_RELATIONSHIP($,$,#17597,#17594)
REPRESENTATION_RELATIONSHIP_WITH_TRANSFORMATION(#22)
SHAPE_REPRESENTATION_RELATIONSHIP()
);
#134=(
REPRESENTATION_RELATIONSHIP($,$,#17598,#17594)
REPRESENTATION_RELATIONSHIP_WITH_TRANSFORMATION(#23)
SHAPE_REPRESENTATION_RELATIONSHIP()
);
#135=(
REPRESENTATION_RELATIONSHIP($,$,#17599,#17594)
REPRESENTATION_RELATIONSHIP_WITH_TRANSFORMATION(#24)
SHAPE_REPRESENTATION_RELATIONSHIP()
);
#136=(
REPRESENTATION_RELATIONSHIP($,$,#17600,#17594)
REPRESENTATION_RELATIONSHIP_WITH_TRANSFORMATION(#25)
SHAPE_REPRESENTATION_RELATIONSHIP()
);
#137=(
REPRESENTATION_RELATIONSHIP($,$,#17600,#17594)
REPRESENTATION_RELATIONSHIP_WITH_TRANSFORMATION(#26)
SHAPE_REPRESENTATION_RELATIONSHIP()
);
#138=(
REPRESENTATION_RELATIONSHIP($,$,#17615,#17614)
REPRESENTATION_RELATIONSHIP_WITH_TRANSFORMATION(#27)
SHAPE_REPRESENTATION_RELATIONSHIP()
);
#139=(
REPRESENTATION_RELATIONSHIP($,$,#17616,#17614)
REPRESENTATION_RELATIONSHIP_WITH_TRANSFORMATION(#28)
SHAPE_REPRESENTATION_RELATIONSHIP()
);
#140=(
REPRESENTATION_RELATIONSHIP($,$,#17560,#17559)
REPRESENTATION_RELATIONSHIP_WITH_TRANSFORMATION(#29)
SHAPE_REPRESENTATION_RELATIONSHIP()
);
#141=(
REPRESENTATION_RELATIONSHIP($,$,#17561,#17559)
REPRESENTATION_RELATIONSHIP_WITH_TRANSFORMATION(#30)
SHAPE_REPRESENTATION_RELATIONSHIP()
);
#142=(
REPRESENTATION_RELATIONSHIP($,$,#17562,#17559)
REPRESENTATION_RELATIONSHIP_WITH_TRANSFORMATION(#31)
SHAPE_REPRESENTATION_RELATIONSHIP()
);
#143=(
REPRESENTATION_RELATIONSHIP($,$,#17563,#17559)
REPRESENTATION_RELATIONSHIP_WITH_TRANSFORMATION(#32)
SHAPE_REPRESENTATION_RELATIONSHIP()
);
#144=(
REPRESENTATION_RELATIONSHIP($,$,#17564,#17559)
REPRESENTATION_RELATIONSHIP_WITH_TRANSFORMATION(#33)
SHAPE_REPRESENTATION_RELATIONSHIP()
);
#145=(
REPRESENTATION_RELATIONSHIP($,$,#17565,#17559)
REPRESENTATION_RELATIONSHIP_WITH_TRANSFORMATION(#34)
SHAPE_REPRESENTATION_RELATIONSHIP()
);
#146=(
REPRESENTATION_RELATIONSHIP($,$,#17566,#17559)
REPRESENTATION_RELATIONSHIP_WITH_TRANSFORMATION(#35)
SHAPE_REPRESENTATION_RELATIONSHIP()
);
#147=(
REPRESENTATION_RELATIONSHIP($,$,#17567,#17559)
REPRESENTATION_RELATIONSHIP_WITH_TRANSFORMATION(#36)
SHAPE_REPRESENTATION_RELATIONSHIP()
);
#148=(
REPRESENTATION_RELATIONSHIP($,$,#17568,#17559)
REPRESENTATION_RELATIONSHIP_WITH_TRANSFORMATION(#37)
SHAPE_REPRESENTATION_RELATIONSHIP()
);
#149=(
REPRESENTATION_RELATIONSHIP($,$,#17569,#17559)
REPRESENTATION_RELATIONSHIP_WITH_TRANSFORMATION(#38)
SHAPE_REPRESENTATION_RELATIONSHIP()
);
#150=(
REPRESENTATION_RELATIONSHIP($,$,#17570,#17559)
REPRESENTATION_RELATIONSHIP_WITH_TRANSFORMATION(#39)
SHAPE_REPRESENTATION_RELATIONSHIP()
);
#151=(
REPRESENTATION_RELATIONSHIP($,$,#17571,#17559)
REPRESENTATION_RELATIONSHIP_WITH_TRANSFORMATION(#40)
SHAPE_REPRESENTATION_RELATIONSHIP()
);
#152=(
REPRESENTATION_RELATIONSHIP($,$,#17571,#17559)
REPRESENTATION_RELATIONSHIP_WITH_TRANSFORMATION(#41)
SHAPE_REPRESENTATION_RELATIONSHIP()
);
#153=(
REPRESENTATION_RELATIONSHIP($,$,#17571,#17559)
REPRESENTATION_RELATIONSHIP_WITH_TRANSFORMATION(#42)
SHAPE_REPRESENTATION_RELATIONSHIP()
);
#154=(
REPRESENTATION_RELATIONSHIP($,$,#17571,#17559)
REPRESENTATION_RELATIONSHIP_WITH_TRANSFORMATION(#43)
SHAPE_REPRESENTATION_RELATIONSHIP()
);
#155=(
REPRESENTATION_RELATIONSHIP($,$,#17572,#17559)
REPRESENTATION_RELATIONSHIP_WITH_TRANSFORMATION(#44)
SHAPE_REPRESENTATION_RELATIONSHIP()
);
#156=(
REPRESENTATION_RELATIONSHIP($,$,#17575,#17559)
REPRESENTATION_RELATIONSHIP_WITH_TRANSFORMATION(#45)
SHAPE_REPRESENTATION_RELATIONSHIP()
);
#157=(
REPRESENTATION_RELATIONSHIP($,$,#17576,#17559)
REPRESENTATION_RELATIONSHIP_WITH_TRANSFORMATION(#46)
SHAPE_REPRESENTATION_RELATIONSHIP()
);
#158=(
REPRESENTATION_RELATIONSHIP($,$,#17575,#17559)
REPRESENTATION_RELATIONSHIP_WITH_TRANSFORMATION(#47)
SHAPE_REPRESENTATION_RELATIONSHIP()
);
#159=(
REPRESENTATION_RELATIONSHIP($,$,#17576,#17559)
REPRESENTATION_RELATIONSHIP_WITH_TRANSFORMATION(#48)
SHAPE_REPRESENTATION_RELATIONSHIP()
);
#160=(
REPRESENTATION_RELATIONSHIP($,$,#17571,#17559)
REPRESENTATION_RELATIONSHIP_WITH_TRANSFORMATION(#49)
SHAPE_REPRESENTATION_RELATIONSHIP()
);
#161=(
REPRESENTATION_RELATIONSHIP($,$,#17571,#17559)
REPRESENTATION_RELATIONSHIP_WITH_TRANSFORMATION(#50)
SHAPE_REPRESENTATION_RELATIONSHIP()
);
#162=(
REPRESENTATION_RELATIONSHIP($,$,#17571,#17559)
REPRESENTATION_RELATIONSHIP_WITH_TRANSFORMATION(#51)
SHAPE_REPRESENTATION_RELATIONSHIP()
);
#163=(
REPRESENTATION_RELATIONSHIP($,$,#17571,#17559)
REPRESENTATION_RELATIONSHIP_WITH_TRANSFORMATION(#52)
SHAPE_REPRESENTATION_RELATIONSHIP()
);
#164=(
REPRESENTATION_RELATIONSHIP($,$,#17572,#17559)
REPRESENTATION_RELATIONSHIP_WITH_TRANSFORMATION(#53)
SHAPE_REPRESENTATION_RELATIONSHIP()
);
#165=(
REPRESENTATION_RELATIONSHIP($,$,#17575,#17559)
REPRESENTATION_RELATIONSHIP_WITH_TRANSFORMATION(#54)
SHAPE_REPRESENTATION_RELATIONSHIP()
);
#166=(
REPRESENTATION_RELATIONSHIP($,$,#17576,#17559)
REPRESENTATION_RELATIONSHIP_WITH_TRANSFORMATION(#55)
SHAPE_REPRESENTATION_RELATIONSHIP()
);
#167=(
REPRESENTATION_RELATIONSHIP($,$,#17575,#17559)
REPRESENTATION_RELATIONSHIP_WITH_TRANSFORMATION(#56)
SHAPE_REPRESENTATION_RELATIONSHIP()
);
#168=(
REPRESENTATION_RELATIONSHIP($,$,#17576,#17559)
REPRESENTATION_RELATIONSHIP_WITH_TRANSFORMATION(#57)
SHAPE_REPRESENTATION_RELATIONSHIP()
);
#169=(
REPRESENTATION_RELATIONSHIP($,$,#17577,#17559)
REPRESENTATION_RELATIONSHIP_WITH_TRANSFORMATION(#58)
SHAPE_REPRESENTATION_RELATIONSHIP()
);
#170=(
REPRESENTATION_RELATIONSHIP($,$,#17578,#17559)
REPRESENTATION_RELATIONSHIP_WITH_TRANSFORMATION(#59)
SHAPE_REPRESENTATION_RELATIONSHIP()
);
#171=(
REPRESENTATION_RELATIONSHIP($,$,#17579,#17559)
REPRESENTATION_RELATIONSHIP_WITH_TRANSFORMATION(#60)
SHAPE_REPRESENTATION_RELATIONSHIP()
);
#172=(
REPRESENTATION_RELATIONSHIP($,$,#17578,#17559)
REPRESENTATION_RELATIONSHIP_WITH_TRANSFORMATION(#61)
SHAPE_REPRESENTATION_RELATIONSHIP()
);
#173=(
REPRESENTATION_RELATIONSHIP($,$,#17579,#17559)
REPRESENTATION_RELATIONSHIP_WITH_TRANSFORMATION(#62)
SHAPE_REPRESENTATION_RELATIONSHIP()
);
#174=(
REPRESENTATION_RELATIONSHIP($,$,#17580,#17559)
REPRESENTATION_RELATIONSHIP_WITH_TRANSFORMATION(#63)
SHAPE_REPRESENTATION_RELATIONSHIP()
);
#175=(
REPRESENTATION_RELATIONSHIP($,$,#17577,#17559)
REPRESENTATION_RELATIONSHIP_WITH_TRANSFORMATION(#64)
SHAPE_REPRESENTATION_RELATIONSHIP()
);
#176=(
REPRESENTATION_RELATIONSHIP($,$,#17578,#17559)
REPRESENTATION_RELATIONSHIP_WITH_TRANSFORMATION(#65)
SHAPE_REPRESENTATION_RELATIONSHIP()
);
#177=(
REPRESENTATION_RELATIONSHIP($,$,#17579,#17559)
REPRESENTATION_RELATIONSHIP_WITH_TRANSFORMATION(#66)
SHAPE_REPRESENTATION_RELATIONSHIP()
);
#178=(
REPRESENTATION_RELATIONSHIP($,$,#17578,#17559)
REPRESENTATION_RELATIONSHIP_WITH_TRANSFORMATION(#67)
SHAPE_REPRESENTATION_RELATIONSHIP()
);
#179=(
REPRESENTATION_RELATIONSHIP($,$,#17579,#17559)
REPRESENTATION_RELATIONSHIP_WITH_TRANSFORMATION(#68)
SHAPE_REPRESENTATION_RELATIONSHIP()
);
#180=(
REPRESENTATION_RELATIONSHIP($,$,#17580,#17559)
REPRESENTATION_RELATIONSHIP_WITH_TRANSFORMATION(#69)
SHAPE_REPRESENTATION_RELATIONSHIP()
);
#181=(
REPRESENTATION_RELATIONSHIP($,$,#17617,#17559)
REPRESENTATION_RELATIONSHIP_WITH_TRANSFORMATION(#70)
SHAPE_REPRESENTATION_RELATIONSHIP()
);
#182=(
REPRESENTATION_RELATIONSHIP($,$,#17617,#17559)
REPRESENTATION_RELATIONSHIP_WITH_TRANSFORMATION(#71)
SHAPE_REPRESENTATION_RELATIONSHIP()
);
#183=(
REPRESENTATION_RELATIONSHIP($,$,#17577,#17559)
REPRESENTATION_RELATIONSHIP_WITH_TRANSFORMATION(#72)
SHAPE_REPRESENTATION_RELATIONSHIP()
);
#184=(
REPRESENTATION_RELATIONSHIP($,$,#17578,#17559)
REPRESENTATION_RELATIONSHIP_WITH_TRANSFORMATION(#73)
SHAPE_REPRESENTATION_RELATIONSHIP()
);
#185=(
REPRESENTATION_RELATIONSHIP($,$,#17579,#17559)
REPRESENTATION_RELATIONSHIP_WITH_TRANSFORMATION(#74)
SHAPE_REPRESENTATION_RELATIONSHIP()
);
#186=(
REPRESENTATION_RELATIONSHIP($,$,#17578,#17559)
REPRESENTATION_RELATIONSHIP_WITH_TRANSFORMATION(#75)
SHAPE_REPRESENTATION_RELATIONSHIP()
);
#187=(
REPRESENTATION_RELATIONSHIP($,$,#17579,#17559)
REPRESENTATION_RELATIONSHIP_WITH_TRANSFORMATION(#76)
SHAPE_REPRESENTATION_RELATIONSHIP()
);
#188=(
REPRESENTATION_RELATIONSHIP($,$,#17580,#17559)
REPRESENTATION_RELATIONSHIP_WITH_TRANSFORMATION(#77)
SHAPE_REPRESENTATION_RELATIONSHIP()
);
#189=(
REPRESENTATION_RELATIONSHIP($,$,#17577,#17559)
REPRESENTATION_RELATIONSHIP_WITH_TRANSFORMATION(#78)
SHAPE_REPRESENTATION_RELATIONSHIP()
);
#190=(
REPRESENTATION_RELATIONSHIP($,$,#17578,#17559)
REPRESENTATION_RELATIONSHIP_WITH_TRANSFORMATION(#79)
SHAPE_REPRESENTATION_RELATIONSHIP()
);
#191=(
REPRESENTATION_RELATIONSHIP($,$,#17579,#17559)
REPRESENTATION_RELATIONSHIP_WITH_TRANSFORMATION(#80)
SHAPE_REPRESENTATION_RELATIONSHIP()
);
#192=(
REPRESENTATION_RELATIONSHIP($,$,#17578,#17559)
REPRESENTATION_RELATIONSHIP_WITH_TRANSFORMATION(#81)
SHAPE_REPRESENTATION_RELATIONSHIP()
);
#193=(
REPRESENTATION_RELATIONSHIP($,$,#17579,#17559)
REPRESENTATION_RELATIONSHIP_WITH_TRANSFORMATION(#82)
SHAPE_REPRESENTATION_RELATIONSHIP()
);
#194=(
REPRESENTATION_RELATIONSHIP($,$,#17580,#17559)
REPRESENTATION_RELATIONSHIP_WITH_TRANSFORMATION(#83)
SHAPE_REPRESENTATION_RELATIONSHIP()
);
#195=(
REPRESENTATION_RELATIONSHIP($,$,#17617,#17559)
REPRESENTATION_RELATIONSHIP_WITH_TRANSFORMATION(#84)
SHAPE_REPRESENTATION_RELATIONSHIP()
);
#196=(
REPRESENTATION_RELATIONSHIP($,$,#17617,#17559)
REPRESENTATION_RELATIONSHIP_WITH_TRANSFORMATION(#85)
SHAPE_REPRESENTATION_RELATIONSHIP()
);
#197=(
REPRESENTATION_RELATIONSHIP($,$,#17581,#17559)
REPRESENTATION_RELATIONSHIP_WITH_TRANSFORMATION(#86)
SHAPE_REPRESENTATION_RELATIONSHIP()
);
#198=(
REPRESENTATION_RELATIONSHIP($,$,#17581,#17559)
REPRESENTATION_RELATIONSHIP_WITH_TRANSFORMATION(#87)
SHAPE_REPRESENTATION_RELATIONSHIP()
);
#199=(
REPRESENTATION_RELATIONSHIP($,$,#17583,#17582)
REPRESENTATION_RELATIONSHIP_WITH_TRANSFORMATION(#88)
SHAPE_REPRESENTATION_RELATIONSHIP()
);
#200=(
REPRESENTATION_RELATIONSHIP($,$,#17584,#17582)
REPRESENTATION_RELATIONSHIP_WITH_TRANSFORMATION(#89)
SHAPE_REPRESENTATION_RELATIONSHIP()
);
#201=(
REPRESENTATION_RELATIONSHIP($,$,#17585,#17582)
REPRESENTATION_RELATIONSHIP_WITH_TRANSFORMATION(#90)
SHAPE_REPRESENTATION_RELATIONSHIP()
);
#202=(
REPRESENTATION_RELATIONSHIP($,$,#17586,#17582)
REPRESENTATION_RELATIONSHIP_WITH_TRANSFORMATION(#91)
SHAPE_REPRESENTATION_RELATIONSHIP()
);
#203=(
REPRESENTATION_RELATIONSHIP($,$,#17587,#17582)
REPRESENTATION_RELATIONSHIP_WITH_TRANSFORMATION(#92)
SHAPE_REPRESENTATION_RELATIONSHIP()
);
#204=(
REPRESENTATION_RELATIONSHIP($,$,#17588,#17582)
REPRESENTATION_RELATIONSHIP_WITH_TRANSFORMATION(#93)
SHAPE_REPRESENTATION_RELATIONSHIP()
);
#205=(
REPRESENTATION_RELATIONSHIP($,$,#17589,#17582)
REPRESENTATION_RELATIONSHIP_WITH_TRANSFORMATION(#94)
SHAPE_REPRESENTATION_RELATIONSHIP()
);
#206=(
REPRESENTATION_RELATIONSHIP($,$,#17590,#17582)
REPRESENTATION_RELATIONSHIP_WITH_TRANSFORMATION(#95)
SHAPE_REPRESENTATION_RELATIONSHIP()
);
#207=(
REPRESENTATION_RELATIONSHIP($,$,#17591,#17582)
REPRESENTATION_RELATIONSHIP_WITH_TRANSFORMATION(#96)
SHAPE_REPRESENTATION_RELATIONSHIP()
);
#208=(
REPRESENTATION_RELATIONSHIP($,$,#17592,#17582)
REPRESENTATION_RELATIONSHIP_WITH_TRANSFORMATION(#97)
SHAPE_REPRESENTATION_RELATIONSHIP()
);
#209=(
REPRESENTATION_RELATIONSHIP($,$,#17593,#17582)
REPRESENTATION_RELATIONSHIP_WITH_TRANSFORMATION(#98)
SHAPE_REPRESENTATION_RELATIONSHIP()
);
#210=(
REPRESENTATION_RELATIONSHIP($,$,#17593,#17582)
REPRESENTATION_RELATIONSHIP_WITH_TRANSFORMATION(#99)
SHAPE_REPRESENTATION_RELATIONSHIP()
);
#211=(
REPRESENTATION_RELATIONSHIP($,$,#17593,#17582)
REPRESENTATION_RELATIONSHIP_WITH_TRANSFORMATION(#100)
SHAPE_REPRESENTATION_RELATIONSHIP()
);
#212=(
REPRESENTATION_RELATIONSHIP($,$,#17617,#17582)
REPRESENTATION_RELATIONSHIP_WITH_TRANSFORMATION(#101)
SHAPE_REPRESENTATION_RELATIONSHIP()
);
#213=(
REPRESENTATION_RELATIONSHIP($,$,#17607,#17606)
REPRESENTATION_RELATIONSHIP_WITH_TRANSFORMATION(#102)
SHAPE_REPRESENTATION_RELATIONSHIP()
);
#214=(
REPRESENTATION_RELATIONSHIP($,$,#17608,#17606)
REPRESENTATION_RELATIONSHIP_WITH_TRANSFORMATION(#103)
SHAPE_REPRESENTATION_RELATIONSHIP()
);
#215=(
REPRESENTATION_RELATIONSHIP($,$,#17609,#17606)
REPRESENTATION_RELATIONSHIP_WITH_TRANSFORMATION(#104)
SHAPE_REPRESENTATION_RELATIONSHIP()
);
#216=(
REPRESENTATION_RELATIONSHIP($,$,#17610,#17606)
REPRESENTATION_RELATIONSHIP_WITH_TRANSFORMATION(#105)
SHAPE_REPRESENTATION_RELATIONSHIP()
);
#217=(
REPRESENTATION_RELATIONSHIP($,$,#17611,#17606)
REPRESENTATION_RELATIONSHIP_WITH_TRANSFORMATION(#106)
SHAPE_REPRESENTATION_RELATIONSHIP()
);
#218=(
REPRESENTATION_RELATIONSHIP($,$,#17612,#17606)
REPRESENTATION_RELATIONSHIP_WITH_TRANSFORMATION(#107)
SHAPE_REPRESENTATION_RELATIONSHIP()
);
#219=(
REPRESENTATION_RELATIONSHIP($,$,#17613,#17606)
REPRESENTATION_RELATIONSHIP_WITH_TRANSFORMATION(#108)
SHAPE_REPRESENTATION_RELATIONSHIP()
);
#220=(
REPRESENTATION_RELATIONSHIP($,$,#17614,#17606)
REPRESENTATION_RELATIONSHIP_WITH_TRANSFORMATION(#109)
SHAPE_REPRESENTATION_RELATIONSHIP()
);
#221=(
REPRESENTATION_RELATIONSHIP($,$,#17614,#17606)
REPRESENTATION_RELATIONSHIP_WITH_TRANSFORMATION(#110)
SHAPE_REPRESENTATION_RELATIONSHIP()
);
#222=(
REPRESENTATION_RELATIONSHIP($,$,#17617,#17606)
REPRESENTATION_RELATIONSHIP_WITH_TRANSFORMATION(#111)
SHAPE_REPRESENTATION_RELATIONSHIP()
);
#223=(
REPRESENTATION_RELATIONSHIP($,$,#17617,#17606)
REPRESENTATION_RELATIONSHIP_WITH_TRANSFORMATION(#112)
SHAPE_REPRESENTATION_RELATIONSHIP()
);
#224=(
REPRESENTATION_RELATIONSHIP($,$,#17617,#17606)
REPRESENTATION_RELATIONSHIP_WITH_TRANSFORMATION(#113)
SHAPE_REPRESENTATION_RELATIONSHIP()
);
#225=(
REPRESENTATION_RELATIONSHIP($,$,#17617,#17606)
REPRESENTATION_RELATIONSHIP_WITH_TRANSFORMATION(#114)
SHAPE_REPRESENTATION_RELATIONSHIP()
);
#226=(
REPRESENTATION_RELATIONSHIP($,$,#17617,#17606)
REPRESENTATION_RELATIONSHIP_WITH_TRANSFORMATION(#115)
SHAPE_REPRESENTATION_RELATIONSHIP()
);
#227=(
REPRESENTATION_RELATIONSHIP($,$,#17617,#17606)
REPRESENTATION_RELATIONSHIP_WITH_TRANSFORMATION(#116)
SHAPE_REPRESENTATION_RELATIONSHIP()
);
#228=(
REPRESENTATION_RELATIONSHIP($,$,#17617,#17606)
REPRESENTATION_RELATIONSHIP_WITH_TRANSFORMATION(#117)
SHAPE_REPRESENTATION_RELATIONSHIP()
);
#229=(
REPRESENTATION_RELATIONSHIP($,$,#17617,#17606)
REPRESENTATION_RELATIONSHIP_WITH_TRANSFORMATION(#118)
SHAPE_REPRESENTATION_RELATIONSHIP()
);
#230=(
REPRESENTATION_RELATIONSHIP($,$,#17617,#17606)
REPRESENTATION_RELATIONSHIP_WITH_TRANSFORMATION(#119)
SHAPE_REPRESENTATION_RELATIONSHIP()
);
#231=(
REPRESENTATION_RELATIONSHIP($,$,#17559,#17558)
REPRESENTATION_RELATIONSHIP_WITH_TRANSFORMATION(#120)
SHAPE_REPRESENTATION_RELATIONSHIP()
);
#232=(
REPRESENTATION_RELATIONSHIP($,$,#17582,#17558)
REPRESENTATION_RELATIONSHIP_WITH_TRANSFORMATION(#121)
SHAPE_REPRESENTATION_RELATIONSHIP()
);
#233=(
REPRESENTATION_RELATIONSHIP($,$,#17594,#17558)
REPRESENTATION_RELATIONSHIP_WITH_TRANSFORMATION(#122)
SHAPE_REPRESENTATION_RELATIONSHIP()
);
#234=(
REPRESENTATION_RELATIONSHIP($,$,#17606,#17558)
REPRESENTATION_RELATIONSHIP_WITH_TRANSFORMATION(#123)
SHAPE_REPRESENTATION_RELATIONSHIP()
);
#235=CONTEXT_DEPENDENT_SHAPE_REPRESENTATION(#124,#17404);
#236=CONTEXT_DEPENDENT_SHAPE_REPRESENTATION(#125,#17405);
#237=CONTEXT_DEPENDENT_SHAPE_REPRESENTATION(#126,#17437);
#238=CONTEXT_DEPENDENT_SHAPE_REPRESENTATION(#127,#17438);
#239=CONTEXT_DEPENDENT_SHAPE_REPRESENTATION(#128,#17439);
#240=CONTEXT_DEPENDENT_SHAPE_REPRESENTATION(#129,#17440);
#241=CONTEXT_DEPENDENT_SHAPE_REPRESENTATION(#130,#17441);
#242=CONTEXT_DEPENDENT_SHAPE_REPRESENTATION(#131,#17442);
#243=CONTEXT_DEPENDENT_SHAPE_REPRESENTATION(#132,#17443);
#244=CONTEXT_DEPENDENT_SHAPE_REPRESENTATION(#133,#17444);
#245=CONTEXT_DEPENDENT_SHAPE_REPRESENTATION(#134,#17445);
#246=CONTEXT_DEPENDENT_SHAPE_REPRESENTATION(#135,#17446);
#247=CONTEXT_DEPENDENT_SHAPE_REPRESENTATION(#136,#17447);
#248=CONTEXT_DEPENDENT_SHAPE_REPRESENTATION(#137,#17448);
#249=CONTEXT_DEPENDENT_SHAPE_REPRESENTATION(#138,#17460);
#250=CONTEXT_DEPENDENT_SHAPE_REPRESENTATION(#139,#17461);
#251=CONTEXT_DEPENDENT_SHAPE_REPRESENTATION(#140,#17463);
#252=CONTEXT_DEPENDENT_SHAPE_REPRESENTATION(#141,#17464);
#253=CONTEXT_DEPENDENT_SHAPE_REPRESENTATION(#142,#17465);
#254=CONTEXT_DEPENDENT_SHAPE_REPRESENTATION(#143,#17466);
#255=CONTEXT_DEPENDENT_SHAPE_REPRESENTATION(#144,#17467);
#256=CONTEXT_DEPENDENT_SHAPE_REPRESENTATION(#145,#17468);
#257=CONTEXT_DEPENDENT_SHAPE_REPRESENTATION(#146,#17469);
#258=CONTEXT_DEPENDENT_SHAPE_REPRESENTATION(#147,#17470);
#259=CONTEXT_DEPENDENT_SHAPE_REPRESENTATION(#148,#17471);
#260=CONTEXT_DEPENDENT_SHAPE_REPRESENTATION(#149,#17472);
#261=CONTEXT_DEPENDENT_SHAPE_REPRESENTATION(#150,#17473);
#262=CONTEXT_DEPENDENT_SHAPE_REPRESENTATION(#151,#17474);
#263=CONTEXT_DEPENDENT_SHAPE_REPRESENTATION(#152,#17475);
#264=CONTEXT_DEPENDENT_SHAPE_REPRESENTATION(#153,#17476);
#265=CONTEXT_DEPENDENT_SHAPE_REPRESENTATION(#154,#17477);
#266=CONTEXT_DEPENDENT_SHAPE_REPRESENTATION(#155,#17478);
#267=CONTEXT_DEPENDENT_SHAPE_REPRESENTATION(#156,#17479);
#268=CONTEXT_DEPENDENT_SHAPE_REPRESENTATION(#157,#17480);
#269=CONTEXT_DEPENDENT_SHAPE_REPRESENTATION(#158,#17481);
#270=CONTEXT_DEPENDENT_SHAPE_REPRESENTATION(#159,#17482);
#271=CONTEXT_DEPENDENT_SHAPE_REPRESENTATION(#160,#17483);
#272=CONTEXT_DEPENDENT_SHAPE_REPRESENTATION(#161,#17484);
#273=CONTEXT_DEPENDENT_SHAPE_REPRESENTATION(#162,#17485);
#274=CONTEXT_DEPENDENT_SHAPE_REPRESENTATION(#163,#17486);
#275=CONTEXT_DEPENDENT_SHAPE_REPRESENTATION(#164,#17487);
#276=CONTEXT_DEPENDENT_SHAPE_REPRESENTATION(#165,#17488);
#277=CONTEXT_DEPENDENT_SHAPE_REPRESENTATION(#166,#17489);
#278=CONTEXT_DEPENDENT_SHAPE_REPRESENTATION(#167,#17490);
#279=CONTEXT_DEPENDENT_SHAPE_REPRESENTATION(#168,#17491);
#280=CONTEXT_DEPENDENT_SHAPE_REPRESENTATION(#169,#17492);
#281=CONTEXT_DEPENDENT_SHAPE_REPRESENTATION(#170,#17493);
#282=CONTEXT_DEPENDENT_SHAPE_REPRESENTATION(#171,#17494);
#283=CONTEXT_DEPENDENT_SHAPE_REPRESENTATION(#172,#17495);
#284=CONTEXT_DEPENDENT_SHAPE_REPRESENTATION(#173,#17496);
#285=CONTEXT_DEPENDENT_SHAPE_REPRESENTATION(#174,#17497);
#286=CONTEXT_DEPENDENT_SHAPE_REPRESENTATION(#175,#17498);
#287=CONTEXT_DEPENDENT_SHAPE_REPRESENTATION(#176,#17499);
#288=CONTEXT_DEPENDENT_SHAPE_REPRESENTATION(#177,#17500);
#289=CONTEXT_DEPENDENT_SHAPE_REPRESENTATION(#178,#17501);
#290=CONTEXT_DEPENDENT_SHAPE_REPRESENTATION(#179,#17502);
#291=CONTEXT_DEPENDENT_SHAPE_REPRESENTATION(#180,#17503);
#292=CONTEXT_DEPENDENT_SHAPE_REPRESENTATION(#181,#17504);
#293=CONTEXT_DEPENDENT_SHAPE_REPRESENTATION(#182,#17505);
#294=CONTEXT_DEPENDENT_SHAPE_REPRESENTATION(#183,#17506);
#295=CONTEXT_DEPENDENT_SHAPE_REPRESENTATION(#184,#17507);
#296=CONTEXT_DEPENDENT_SHAPE_REPRESENTATION(#185,#17508);
#297=CONTEXT_DEPENDENT_SHAPE_REPRESENTATION(#186,#17509);
#298=CONTEXT_DEPENDENT_SHAPE_REPRESENTATION(#187,#17510);
#299=CONTEXT_DEPENDENT_SHAPE_REPRESENTATION(#188,#17511);
#300=CONTEXT_DEPENDENT_SHAPE_REPRESENTATION(#189,#17512);
#301=CONTEXT_DEPENDENT_SHAPE_REPRESENTATION(#190,#17513);
#302=CONTEXT_DEPENDENT_SHAPE_REPRESENTATION(#191,#17514);
#303=CONTEXT_DEPENDENT_SHAPE_REPRESENTATION(#192,#17515);
#304=CONTEXT_DEPENDENT_SHAPE_REPRESENTATION(#193,#17516);
#305=CONTEXT_DEPENDENT_SHAPE_REPRESENTATION(#194,#17517);
#306=CONTEXT_DEPENDENT_SHAPE_REPRESENTATION(#195,#17518);
#307=CONTEXT_DEPENDENT_SHAPE_REPRESENTATION(#196,#17519);
#308=CONTEXT_DEPENDENT_SHAPE_REPRESENTATION(#197,#17520);
#309=CONTEXT_DEPENDENT_SHAPE_REPRESENTATION(#198,#17521);
#310=CONTEXT_DEPENDENT_SHAPE_REPRESENTATION(#199,#17522);
#311=CONTEXT_DEPENDENT_SHAPE_REPRESENTATION(#200,#17523);
#312=CONTEXT_DEPENDENT_SHAPE_REPRESENTATION(#201,#17524);
#313=CONTEXT_DEPENDENT_SHAPE_REPRESENTATION(#202,#17525);
#314=CONTEXT_DEPENDENT_SHAPE_REPRESENTATION(#203,#17526);
#315=CONTEXT_DEPENDENT_SHAPE_REPRESENTATION(#204,#17527);
#316=CONTEXT_DEPENDENT_SHAPE_REPRESENTATION(#205,#17528);
#317=CONTEXT_DEPENDENT_SHAPE_REPRESENTATION(#206,#17529);
#318=CONTEXT_DEPENDENT_SHAPE_REPRESENTATION(#207,#17530);
#319=CONTEXT_DEPENDENT_SHAPE_REPRESENTATION(#208,#17531);
#320=CONTEXT_DEPENDENT_SHAPE_REPRESENTATION(#209,#17532);
#321=CONTEXT_DEPENDENT_SHAPE_REPRESENTATION(#210,#17533);
#322=CONTEXT_DEPENDENT_SHAPE_REPRESENTATION(#211,#17534);
#323=CONTEXT_DEPENDENT_SHAPE_REPRESENTATION(#212,#17535);
#324=CONTEXT_DEPENDENT_SHAPE_REPRESENTATION(#213,#17536);
#325=CONTEXT_DEPENDENT_SHAPE_REPRESENTATION(#214,#17537);
#326=CONTEXT_DEPENDENT_SHAPE_REPRESENTATION(#215,#17538);
#327=CONTEXT_DEPENDENT_SHAPE_REPRESENTATION(#216,#17539);
#328=CONTEXT_DEPENDENT_SHAPE_REPRESENTATION(#217,#17540);
#329=CONTEXT_DEPENDENT_SHAPE_REPRESENTATION(#218,#17541);
#330=CONTEXT_DEPENDENT_SHAPE_REPRESENTATION(#219,#17542);
#331=CONTEXT_DEPENDENT_SHAPE_REPRESENTATION(#220,#17543);
#332=CONTEXT_DEPENDENT_SHAPE_REPRESENTATION(#221,#17544);
#333=CONTEXT_DEPENDENT_SHAPE_REPRESENTATION(#222,#17545);
#334=CONTEXT_DEPENDENT_SHAPE_REPRESENTATION(#223,#17546);
#335=CONTEXT_DEPENDENT_SHAPE_REPRESENTATION(#224,#17547);
#336=CONTEXT_DEPENDENT_SHAPE_REPRESENTATION(#225,#17548);
#337=CONTEXT_DEPENDENT_SHAPE_REPRESENTATION(#226,#17549);
#338=CONTEXT_DEPENDENT_SHAPE_REPRESENTATION(#227,#17550);
#339=CONTEXT_DEPENDENT_SHAPE_REPRESENTATION(#228,#17551);
#340=CONTEXT_DEPENDENT_SHAPE_REPRESENTATION(#229,#17552);
#341=CONTEXT_DEPENDENT_SHAPE_REPRESENTATION(#230,#17553);
#342=CONTEXT_DEPENDENT_SHAPE_REPRESENTATION(#231,#17554);
#343=CONTEXT_DEPENDENT_SHAPE_REPRESENTATION(#232,#17555);
#344=CONTEXT_DEPENDENT_SHAPE_REPRESENTATION(#233,#17556);
#345=CONTEXT_DEPENDENT_SHAPE_REPRESENTATION(#234,#17557);
#346=NEXT_ASSEMBLY_USAGE_OCCURRENCE('Housing:1','Housing:1','Housing:1',
#17633,#17634,'Housing:1');
#347=NEXT_ASSEMBLY_USAGE_OCCURRENCE('Insert bearing:1',
'Insert bearing:1','Insert bearing:1',#17633,#17635,'Insert bearing:1');
#348=NEXT_ASSEMBLY_USAGE_OCCURRENCE('Inner ring:1','Inner ring:1',
'Inner ring:1',#17661,#17662,'Inner ring:1');
#349=NEXT_ASSEMBLY_USAGE_OCCURRENCE('Outer ring:1','Outer ring:1',
'Outer ring:1',#17661,#17663,'Outer ring:1');
#350=NEXT_ASSEMBLY_USAGE_OCCURRENCE('Balls:1','Balls:1','Balls:1',#17661,
#17664,'Balls:1');
#351=NEXT_ASSEMBLY_USAGE_OCCURRENCE('Cage:1','Cage:1','Cage:1',#17661,#17665,
'Cage:1');
#352=NEXT_ASSEMBLY_USAGE_OCCURRENCE('Seals 2RS:1','Seals 2RS:1',
'Seals 2RS:1',#17661,#17666,'Seals 2RS:1');
#353=NEXT_ASSEMBLY_USAGE_OCCURRENCE('Connecting rod:1',
'Connecting rod:1','Connecting rod:1',#17655,#17656,'Connecting rod:1');
#354=NEXT_ASSEMBLY_USAGE_OCCURRENCE('Rod bearing retainer:1',
'Rod bearing retainer:1','Rod bearing retainer:1',#17655,#17657,
'Rod bearing retainer:1');
#355=NEXT_ASSEMBLY_USAGE_OCCURRENCE('Rod bearing retainer (1):1',
'Rod bearing retainer (1):1','Rod bearing retainer (1):1',#17655,#17658,
'Rod bearing retainer (1):1');
#356=NEXT_ASSEMBLY_USAGE_OCCURRENCE('Rod bearing retainer (2):1',
'Rod bearing retainer (2):1','Rod bearing retainer (2):1',#17655,#17659,
'Rod bearing retainer (2):1');
#357=NEXT_ASSEMBLY_USAGE_OCCURRENCE('Rod bearing retainer (3):1',
'Rod bearing retainer (3):1','Rod bearing retainer (3):1',#17655,#17660,
'Rod bearing retainer (3):1');
#358=NEXT_ASSEMBLY_USAGE_OCCURRENCE(
'Sealed Ball Bearing - 10 x 30 x 9 mm:2',
'Sealed Ball Bearing - 10 x 30 x 9 mm:2',
'Sealed Ball Bearing - 10 x 30 x 9 mm:2',#17655,#17661,
'Sealed Ball Bearing - 10 x 30 x 9 mm:2');
#359=NEXT_ASSEMBLY_USAGE_OCCURRENCE(
'Sealed Ball Bearing - 10 x 30 x 9 mm:3',
'Sealed Ball Bearing - 10 x 30 x 9 mm:3',
'Sealed Ball Bearing - 10 x 30 x 9 mm:3',#17655,#17661,
'Sealed Ball Bearing - 10 x 30 x 9 mm:3');
#360=NEXT_ASSEMBLY_USAGE_OCCURRENCE('Steel sleeve:1','Steel sleeve:1',
'Steel sleeve:1',#17675,#17676,'Steel sleeve:1');
#361=NEXT_ASSEMBLY_USAGE_OCCURRENCE('Ball retainer (plastic):1',
'Ball retainer (plastic):1','Ball retainer (plastic):1',#17675,#17677,
'Ball retainer (plastic):1');
#362=NEXT_ASSEMBLY_USAGE_OCCURRENCE('Base:1','Base:1','Base:1',#17620,#17621,
'Base:1');
#363=NEXT_ASSEMBLY_USAGE_OCCURRENCE('Bearing pedestal:1',
'Bearing pedestal:1','Bearing pedestal:1',#17620,#17622,
'Bearing pedestal:1');
#364=NEXT_ASSEMBLY_USAGE_OCCURRENCE('Bearing bolt reducer:1',
'Bearing bolt reducer:1','Bearing bolt reducer:1',#17620,#17623,
'Bearing bolt reducer:1');
#365=NEXT_ASSEMBLY_USAGE_OCCURRENCE('Bearing bolt reducer (1):1',
'Bearing bolt reducer (1):1','Bearing bolt reducer (1):1',#17620,#17624,
'Bearing bolt reducer (1):1');
#366=NEXT_ASSEMBLY_USAGE_OCCURRENCE('Bearing pedestal (1):1',
'Bearing pedestal (1):1','Bearing pedestal (1):1',#17620,#17625,
'Bearing pedestal (1):1');
#367=NEXT_ASSEMBLY_USAGE_OCCURRENCE('Bearing bolt reducer (2):1',
'Bearing bolt reducer (2):1','Bearing bolt reducer (2):1',#17620,#17626,
'Bearing bolt reducer (2):1');
#368=NEXT_ASSEMBLY_USAGE_OCCURRENCE('Bearing bolt reducer (3):1',
'Bearing bolt reducer (3):1','Bearing bolt reducer (3):1',#17620,#17627,
'Bearing bolt reducer (3):1');
#369=NEXT_ASSEMBLY_USAGE_OCCURRENCE('Guide pedestal:1',
'Guide pedestal:1','Guide pedestal:1',#17620,#17628,'Guide pedestal:1');
#370=NEXT_ASSEMBLY_USAGE_OCCURRENCE('Guide pedestal (1):1',
'Guide pedestal (1):1','Guide pedestal (1):1',#17620,#17629,
'Guide pedestal (1):1');
#371=NEXT_ASSEMBLY_USAGE_OCCURRENCE('Foot strip:1','Foot strip:1',
'Foot strip:1',#17620,#17630,'Foot strip:1');
#372=NEXT_ASSEMBLY_USAGE_OCCURRENCE('Foot strip (1):1',
'Foot strip (1):1','Foot strip (1):1',#17620,#17631,'Foot strip (1):1');
#373=NEXT_ASSEMBLY_USAGE_OCCURRENCE('Cap Screw - M5x20:2',
'Cap Screw - M5x20:2','Cap Screw - M5x20:2',#17620,#17632,
'Cap Screw - M5x20:2');
#374=NEXT_ASSEMBLY_USAGE_OCCURRENCE('Cap Screw - M5x20:3',
'Cap Screw - M5x20:3','Cap Screw - M5x20:3',#17620,#17632,
'Cap Screw - M5x20:3');
#375=NEXT_ASSEMBLY_USAGE_OCCURRENCE('Cap Screw - M5x20:4',
'Cap Screw - M5x20:4','Cap Screw - M5x20:4',#17620,#17632,
'Cap Screw - M5x20:4');
#376=NEXT_ASSEMBLY_USAGE_OCCURRENCE('Cap Screw - M5x20:5',
'Cap Screw - M5x20:5','Cap Screw - M5x20:5',#17620,#17632,
'Cap Screw - M5x20:5');
#377=NEXT_ASSEMBLY_USAGE_OCCURRENCE(
'Pillow Block Bearing - 20 mm Bore:2',
'Pillow Block Bearing - 20 mm Bore:2',
'Pillow Block Bearing - 20 mm Bore:2',#17620,#17633,
'Pillow Block Bearing - 20 mm Bore:2');
#378=NEXT_ASSEMBLY_USAGE_OCCURRENCE('Flat Washer - M8:2',
'Flat Washer - M8:2','Flat Washer - M8:2',#17620,#17636,
'Flat Washer - M8:2');
#379=NEXT_ASSEMBLY_USAGE_OCCURRENCE('M8x25 Bolt:2','M8x25 Bolt:2',
'M8x25 Bolt:2',#17620,#17637,'M8x25 Bolt:2');
#380=NEXT_ASSEMBLY_USAGE_OCCURRENCE('Flat Washer - M8:3',
'Flat Washer - M8:3','Flat Washer - M8:3',#17620,#17636,
'Flat Washer - M8:3');
#381=NEXT_ASSEMBLY_USAGE_OCCURRENCE('M8x25 Bolt:3','M8x25 Bolt:3',
'M8x25 Bolt:3',#17620,#17637,'M8x25 Bolt:3');
#382=NEXT_ASSEMBLY_USAGE_OCCURRENCE('Cap Screw - M5x20:6',
'Cap Screw - M5x20:6','Cap Screw - M5x20:6',#17620,#17632,
'Cap Screw - M5x20:6');
#383=NEXT_ASSEMBLY_USAGE_OCCURRENCE('Cap Screw - M5x20:7',
'Cap Screw - M5x20:7','Cap Screw - M5x20:7',#17620,#17632,
'Cap Screw - M5x20:7');
#384=NEXT_ASSEMBLY_USAGE_OCCURRENCE('Cap Screw - M5x20:8',
'Cap Screw - M5x20:8','Cap Screw - M5x20:8',#17620,#17632,
'Cap Screw - M5x20:8');
#385=NEXT_ASSEMBLY_USAGE_OCCURRENCE('Cap Screw - M5x20:9',
'Cap Screw - M5x20:9','Cap Screw - M5x20:9',#17620,#17632,
'Cap Screw - M5x20:9');
#386=NEXT_ASSEMBLY_USAGE_OCCURRENCE(
'Pillow Block Bearing - 20 mm Bore:3',
'Pillow Block Bearing - 20 mm Bore:3',
'Pillow Block Bearing - 20 mm Bore:3',#17620,#17633,
'Pillow Block Bearing - 20 mm Bore:3');
#387=NEXT_ASSEMBLY_USAGE_OCCURRENCE('Flat Washer - M8:4',
'Flat Washer - M8:4','Flat Washer - M8:4',#17620,#17636,
'Flat Washer - M8:4');
#388=NEXT_ASSEMBLY_USAGE_OCCURRENCE('M8x25 Bolt:4','M8x25 Bolt:4',
'M8x25 Bolt:4',#17620,#17637,'M8x25 Bolt:4');
#389=NEXT_ASSEMBLY_USAGE_OCCURRENCE('Flat Washer - M8:5',
'Flat Washer - M8:5','Flat Washer - M8:5',#17620,#17636,
'Flat Washer - M8:5');
#390=NEXT_ASSEMBLY_USAGE_OCCURRENCE('M8x25 Bolt:5','M8x25 Bolt:5',
'M8x25 Bolt:5',#17620,#17637,'M8x25 Bolt:5');
#391=NEXT_ASSEMBLY_USAGE_OCCURRENCE('Shaft Support - 12 mm Bore:2',
'Shaft Support - 12 mm Bore:2','Shaft Support - 12 mm Bore:2',#17620,#17638,
'Shaft Support - 12 mm Bore:2');
#392=NEXT_ASSEMBLY_USAGE_OCCURRENCE('Flat Washer - M5:2',
'Flat Washer - M5:2','Flat Washer - M5:2',#17620,#17639,
'Flat Washer - M5:2');
#393=NEXT_ASSEMBLY_USAGE_OCCURRENCE('M5x14 Cap Screw:2',
'M5x14 Cap Screw:2','M5x14 Cap Screw:2',#17620,#17640,
'M5x14 Cap Screw:2');
#394=NEXT_ASSEMBLY_USAGE_OCCURRENCE('Flat Washer - M5:3',
'Flat Washer - M5:3','Flat Washer - M5:3',#17620,#17639,
'Flat Washer - M5:3');
#395=NEXT_ASSEMBLY_USAGE_OCCURRENCE('M5x14 Cap Screw:3',
'M5x14 Cap Screw:3','M5x14 Cap Screw:3',#17620,#17640,
'M5x14 Cap Screw:3');
#396=NEXT_ASSEMBLY_USAGE_OCCURRENCE('Cap Screw - M4x16:2',
'Cap Screw - M4x16:2','Cap Screw - M4x16:2',#17620,#17641,
'Cap Screw - M4x16:2');
#397=NEXT_ASSEMBLY_USAGE_OCCURRENCE('Shaft Support - 12 mm Bore:3',
'Shaft Support - 12 mm Bore:3','Shaft Support - 12 mm Bore:3',#17620,#17638,
'Shaft Support - 12 mm Bore:3');
#398=NEXT_ASSEMBLY_USAGE_OCCURRENCE('Flat Washer - M5:4',
'Flat Washer - M5:4','Flat Washer - M5:4',#17620,#17639,
'Flat Washer - M5:4');
#399=NEXT_ASSEMBLY_USAGE_OCCURRENCE('M5x14 Cap Screw:4',
'M5x14 Cap Screw:4','M5x14 Cap Screw:4',#17620,#17640,
'M5x14 Cap Screw:4');
#400=NEXT_ASSEMBLY_USAGE_OCCURRENCE('Flat Washer - M5:5',
'Flat Washer - M5:5','Flat Washer - M5:5',#17620,#17639,
'Flat Washer - M5:5');
#401=NEXT_ASSEMBLY_USAGE_OCCURRENCE('M5x14 Cap Screw:5',
'M5x14 Cap Screw:5','M5x14 Cap Screw:5',#17620,#17640,
'M5x14 Cap Screw:5');
#402=NEXT_ASSEMBLY_USAGE_OCCURRENCE('Cap Screw - M4x16:3',
'Cap Screw - M4x16:3','Cap Screw - M4x16:3',#17620,#17641,
'Cap Screw - M4x16:3');
#403=NEXT_ASSEMBLY_USAGE_OCCURRENCE('M4x10 Cap Screw:2',
'M4x10 Cap Screw:2','M4x10 Cap Screw:2',#17620,#17678,
'M4x10 Cap Screw:2');
#404=NEXT_ASSEMBLY_USAGE_OCCURRENCE('M4x10 Cap Screw:3',
'M4x10 Cap Screw:3','M4x10 Cap Screw:3',#17620,#17678,
'M4x10 Cap Screw:3');
#405=NEXT_ASSEMBLY_USAGE_OCCURRENCE('Shaft Support - 12 mm Bore:4',
'Shaft Support - 12 mm Bore:4','Shaft Support - 12 mm Bore:4',#17620,#17638,
'Shaft Support - 12 mm Bore:4');
#406=NEXT_ASSEMBLY_USAGE_OCCURRENCE('Flat Washer - M5:6',
'Flat Washer - M5:6','Flat Washer - M5:6',#17620,#17639,
'Flat Washer - M5:6');
#407=NEXT_ASSEMBLY_USAGE_OCCURRENCE('M5x14 Cap Screw:6',
'M5x14 Cap Screw:6','M5x14 Cap Screw:6',#17620,#17640,
'M5x14 Cap Screw:6');
#408=NEXT_ASSEMBLY_USAGE_OCCURRENCE('Flat Washer - M5:7',
'Flat Washer - M5:7','Flat Washer - M5:7',#17620,#17639,
'Flat Washer - M5:7');
#409=NEXT_ASSEMBLY_USAGE_OCCURRENCE('M5x14 Cap Screw:7',
'M5x14 Cap Screw:7','M5x14 Cap Screw:7',#17620,#17640,
'M5x14 Cap Screw:7');
#410=NEXT_ASSEMBLY_USAGE_OCCURRENCE('Cap Screw - M4x16:4',
'Cap Screw - M4x16:4','Cap Screw - M4x16:4',#17620,#17641,
'Cap Screw - M4x16:4');
#411=NEXT_ASSEMBLY_USAGE_OCCURRENCE('Shaft Support - 12 mm Bore:5',
'Shaft Support - 12 mm Bore:5','Shaft Support - 12 mm Bore:5',#17620,#17638,
'Shaft Support - 12 mm Bore:5');
#412=NEXT_ASSEMBLY_USAGE_OCCURRENCE('Flat Washer - M5:8',
'Flat Washer - M5:8','Flat Washer - M5:8',#17620,#17639,
'Flat Washer - M5:8');
#413=NEXT_ASSEMBLY_USAGE_OCCURRENCE('M5x14 Cap Screw:8',
'M5x14 Cap Screw:8','M5x14 Cap Screw:8',#17620,#17640,
'M5x14 Cap Screw:8');
#414=NEXT_ASSEMBLY_USAGE_OCCURRENCE('Flat Washer - M5:9',
'Flat Washer - M5:9','Flat Washer - M5:9',#17620,#17639,
'Flat Washer - M5:9');
#415=NEXT_ASSEMBLY_USAGE_OCCURRENCE('M5x14 Cap Screw:9',
'M5x14 Cap Screw:9','M5x14 Cap Screw:9',#17620,#17640,
'M5x14 Cap Screw:9');
#416=NEXT_ASSEMBLY_USAGE_OCCURRENCE('Cap Screw - M4x16:5',
'Cap Screw - M4x16:5','Cap Screw - M4x16:5',#17620,#17641,
'Cap Screw - M4x16:5');
#417=NEXT_ASSEMBLY_USAGE_OCCURRENCE('M4x10 Cap Screw:4',
'M4x10 Cap Screw:4','M4x10 Cap Screw:4',#17620,#17678,
'M4x10 Cap Screw:4');
#418=NEXT_ASSEMBLY_USAGE_OCCURRENCE('M4x10 Cap Screw:5',
'M4x10 Cap Screw:5','M4x10 Cap Screw:5',#17620,#17678,
'M4x10 Cap Screw:5');
#419=NEXT_ASSEMBLY_USAGE_OCCURRENCE('Guide shaft 200 mm:2',
'Guide shaft 200 mm:2','Guide shaft 200 mm:2',#17620,#17642,
'Guide shaft 200 mm:2');
#420=NEXT_ASSEMBLY_USAGE_OCCURRENCE('Guide shaft 200 mm:3',
'Guide shaft 200 mm:3','Guide shaft 200 mm:3',#17620,#17642,
'Guide shaft 200 mm:3');
#421=NEXT_ASSEMBLY_USAGE_OCCURRENCE('Flywheel shaft:1',
'Flywheel shaft:1','Flywheel shaft:1',#17643,#17644,'Flywheel shaft:1');
#422=NEXT_ASSEMBLY_USAGE_OCCURRENCE('Shaft collar:1','Shaft collar:1',
'Shaft collar:1',#17643,#17645,'Shaft collar:1');
#423=NEXT_ASSEMBLY_USAGE_OCCURRENCE('Shaft collar (1):1',
'Shaft collar (1):1','Shaft collar (1):1',#17643,#17646,
'Shaft collar (1):1');
#424=NEXT_ASSEMBLY_USAGE_OCCURRENCE('Rear bearing spacer:1',
'Rear bearing spacer:1','Rear bearing spacer:1',#17643,#17647,
'Rear bearing spacer:1');
#425=NEXT_ASSEMBLY_USAGE_OCCURRENCE('Flywheel:1','Flywheel:1',
'Flywheel:1',#17643,#17648,'Flywheel:1');
#426=NEXT_ASSEMBLY_USAGE_OCCURRENCE('Crank pin:1','Crank pin:1',
'Crank pin:1',#17643,#17649,'Crank pin:1');
#427=NEXT_ASSEMBLY_USAGE_OCCURRENCE('Pin spacer 10 mm:1',
'Pin spacer 10 mm:1','Pin spacer 10 mm:1',#17643,#17650,
'Pin spacer 10 mm:1');
#428=NEXT_ASSEMBLY_USAGE_OCCURRENCE('Pin spacer 4 mm:1',
'Pin spacer 4 mm:1','Pin spacer 4 mm:1',#17643,#17651,
'Pin spacer 4 mm:1');
#429=NEXT_ASSEMBLY_USAGE_OCCURRENCE('Pin keeper:1','Pin keeper:1',
'Pin keeper:1',#17643,#17652,'Pin keeper:1');
#430=NEXT_ASSEMBLY_USAGE_OCCURRENCE('Key 6x6x20:2','Key 6x6x20:2',
'Key 6x6x20:2',#17643,#17653,'Key 6x6x20:2');
#431=NEXT_ASSEMBLY_USAGE_OCCURRENCE('Socket Set Screw - M5x8:2',
'Socket Set Screw - M5x8:2','Socket Set Screw - M5x8:2',#17643,#17654,
'Socket Set Screw - M5x8:2');
#432=NEXT_ASSEMBLY_USAGE_OCCURRENCE('Socket Set Screw - M5x8:3',
'Socket Set Screw - M5x8:3','Socket Set Screw - M5x8:3',#17643,#17654,
'Socket Set Screw - M5x8:3');
#433=NEXT_ASSEMBLY_USAGE_OCCURRENCE('Socket Set Screw - M5x8:4',
'Socket Set Screw - M5x8:4','Socket Set Screw - M5x8:4',#17643,#17654,
'Socket Set Screw - M5x8:4');
#434=NEXT_ASSEMBLY_USAGE_OCCURRENCE('M4x10 Cap Screw:14',
'M4x10 Cap Screw:14','M4x10 Cap Screw:14',#17643,#17678,
'M4x10 Cap Screw:14');
#435=NEXT_ASSEMBLY_USAGE_OCCURRENCE('Slider housing:1',
'Slider housing:1','Slider housing:1',#17667,#17668,'Slider housing:1');
#436=NEXT_ASSEMBLY_USAGE_OCCURRENCE('Bushing cap:1','Bushing cap:1',
'Bushing cap:1',#17667,#17669,'Bushing cap:1');
#437=NEXT_ASSEMBLY_USAGE_OCCURRENCE('Bushing cap (1):1',
'Bushing cap (1):1','Bushing cap (1):1',#17667,#17670,
'Bushing cap (1):1');
#438=NEXT_ASSEMBLY_USAGE_OCCURRENCE('Slider pin:1','Slider pin:1',
'Slider pin:1',#17667,#17671,'Slider pin:1');
#439=NEXT_ASSEMBLY_USAGE_OCCURRENCE('Pin spacer 2 mm:1',
'Pin spacer 2 mm:1','Pin spacer 2 mm:1',#17667,#17672,
'Pin spacer 2 mm:1');
#440=NEXT_ASSEMBLY_USAGE_OCCURRENCE('Pin spacer 4 mm (1):1',
'Pin spacer 4 mm (1):1','Pin spacer 4 mm (1):1',#17667,#17673,
'Pin spacer 4 mm (1):1');
#441=NEXT_ASSEMBLY_USAGE_OCCURRENCE('Pin keeper (1):1',
'Pin keeper (1):1','Pin keeper (1):1',#17667,#17674,'Pin keeper (1):1');
#442=NEXT_ASSEMBLY_USAGE_OCCURRENCE(
'Linear Ball Bushing - 12 x 21 x 30 mm:2',
'Linear Ball Bushing - 12 x 21 x 30 mm:2',
'Linear Ball Bushing - 12 x 21 x 30 mm:2',#17667,#17675,
'Linear Ball Bushing - 12 x 21 x 30 mm:2');
#443=NEXT_ASSEMBLY_USAGE_OCCURRENCE(
'Linear Ball Bushing - 12 x 21 x 30 mm:3',
'Linear Ball Bushing - 12 x 21 x 30 mm:3',
'Linear Ball Bushing - 12 x 21 x 30 mm:3',#17667,#17675,
'Linear Ball Bushing - 12 x 21 x 30 mm:3');
#444=NEXT_ASSEMBLY_USAGE_OCCURRENCE('M4x10 Cap Screw:6',
'M4x10 Cap Screw:6','M4x10 Cap Screw:6',#17667,#17678,
'M4x10 Cap Screw:6');
#445=NEXT_ASSEMBLY_USAGE_OCCURRENCE('M4x10 Cap Screw:7',
'M4x10 Cap Screw:7','M4x10 Cap Screw:7',#17667,#17678,
'M4x10 Cap Screw:7');
#446=NEXT_ASSEMBLY_USAGE_OCCURRENCE('M4x10 Cap Screw:8',
'M4x10 Cap Screw:8','M4x10 Cap Screw:8',#17667,#17678,
'M4x10 Cap Screw:8');
#447=NEXT_ASSEMBLY_USAGE_OCCURRENCE('M4x10 Cap Screw:9',
'M4x10 Cap Screw:9','M4x10 Cap Screw:9',#17667,#17678,
'M4x10 Cap Screw:9');
#448=NEXT_ASSEMBLY_USAGE_OCCURRENCE('M4x10 Cap Screw:10',
'M4x10 Cap Screw:10','M4x10 Cap Screw:10',#17667,#17678,
'M4x10 Cap Screw:10');
#449=NEXT_ASSEMBLY_USAGE_OCCURRENCE('M4x10 Cap Screw:11',
'M4x10 Cap Screw:11','M4x10 Cap Screw:11',#17667,#17678,
'M4x10 Cap Screw:11');
#450=NEXT_ASSEMBLY_USAGE_OCCURRENCE('M4x10 Cap Screw:12',
'M4x10 Cap Screw:12','M4x10 Cap Screw:12',#17667,#17678,
'M4x10 Cap Screw:12');
#451=NEXT_ASSEMBLY_USAGE_OCCURRENCE('M4x10 Cap Screw:13',
'M4x10 Cap Screw:13','M4x10 Cap Screw:13',#17667,#17678,
'M4x10 Cap Screw:13');
#452=NEXT_ASSEMBLY_USAGE_OCCURRENCE('M4x10 Cap Screw:15',
'M4x10 Cap Screw:15','M4x10 Cap Screw:15',#17667,#17678,
'M4x10 Cap Screw:15');
#453=NEXT_ASSEMBLY_USAGE_OCCURRENCE('Bearing and guide frame:1',
'Bearing and guide frame:1','Bearing and guide frame:1',#17619,#17620,
'Bearing and guide frame:1');
#454=NEXT_ASSEMBLY_USAGE_OCCURRENCE('Flywheel and crank:1',
'Flywheel and crank:1','Flywheel and crank:1',#17619,#17643,
'Flywheel and crank:1');
#455=NEXT_ASSEMBLY_USAGE_OCCURRENCE('Connecting rod (1):1',
'Connecting rod (1):1','Connecting rod (1):1',#17619,#17655,
'Connecting rod (1):1');
#456=NEXT_ASSEMBLY_USAGE_OCCURRENCE('Guided slider:1','Guided slider:1',
'Guided slider:1',#17619,#17667,'Guided slider:1');
#457=B_SPLINE_CURVE_WITH_KNOTS('',3,(#14534,#14535,#14536,#14537,#14538,
#14539,#14540,#14541,#14542,#14543),.UNSPECIFIED.,.F.,.F.,(4,2,2,2,4),(1.13193471301885,
1.22626174930539,1.32058878559194,1.41491753480854,1.50924628402513),
 .UNSPECIFIED.);
#458=B_SPLINE_CURVE_WITH_KNOTS('',3,(#14545,#14546,#14547,#14548,#14549,
#14550,#14551,#14552,#14553,#14554,#14555,#14556,#14557,#14558,#14559,#14560,
#14561,#14562),.UNSPECIFIED.,.F.,.F.,(4,2,2,2,2,2,2,2,4),(0.377311571006283,
0.471638607292829,0.565965643579376,0.66029439279597,0.754623142012565,
0.84895189122916,0.943280640445754,1.0376076767323,1.13193471301885),
 .UNSPECIFIED.);
#459=B_SPLINE_CURVE_WITH_KNOTS('',3,(#14563,#14564,#14565,#14566,#14567,
#14568,#14569,#14570,#14571,#14572),.UNSPECIFIED.,.F.,.F.,(4,2,2,2,4),(1.50924628402513,
1.60357503324173,1.69790378245832,1.79223081874487,1.88655785503141),
 .UNSPECIFIED.);
#460=B_SPLINE_CURVE_WITH_KNOTS('',3,(#14575,#14576,#14577,#14578,#14579,
#14580,#14581,#14582,#14583,#14584,#14585,#14586,#14587,#14588,#14589,#14590,
#14591,#14592,#14593,#14594,#14595,#14596,#14597,#14598,#14599,#14600,#14601,
#14602,#14603,#14604,#14605,#14606,#14607,#14608),.UNSPECIFIED.,.T.,.F.,
(4,2,2,2,2,2,2,2,2,2,2,2,2,2,2,2,4),(0.,0.0946120580087934,0.189224116017587,
0.283822945575014,0.378421775132442,0.47302060468987,0.567619434247297,
0.662231492256091,0.756843550264884,0.851455608273677,0.94606766628247,
1.0406664958399,1.13526532539733,1.22986415495475,1.32446298451218,1.41907504252097,
1.51368710052977),.UNSPECIFIED.);
#461=B_SPLINE_CURVE_WITH_KNOTS('',3,(#14611,#14612,#14613,#14614,#14615,
#14616,#14617,#14618,#14619,#14620,#14621,#14622,#14623,#14624,#14625,#14626,
#14627,#14628,#14629,#14630,#14631,#14632,#14633,#14634,#14635,#14636,#14637,
#14638,#14639,#14640,#14641,#14642,#14643,#14644),.UNSPECIFIED.,.T.,.F.,
(4,2,2,2,2,2,2,2,2,2,2,2,2,2,2,2,4),(0.,0.0946120580087934,0.189224116017587,
0.283822945575014,0.378421775132442,0.47302060468987,0.567619434247297,
0.66223149225609,0.756843550264884,0.851455608273677,0.94606766628247,1.0406664958399,
1.13526532539733,1.22986415495475,1.32446298451218,1.41907504252097,1.51368710052977),
 .UNSPECIFIED.);
#462=B_SPLINE_CURVE_WITH_KNOTS('',3,(#14648,#14649,#14650,#14651,#14652,
#14653,#14654,#14655,#14656,#14657),.UNSPECIFIED.,.F.,.F.,(4,2,2,2,4),(1.13193471301885,
1.22626174930539,1.32058878559194,1.41491753480854,1.50924628402513),
 .UNSPECIFIED.);
#463=B_SPLINE_CURVE_WITH_KNOTS('',3,(#14659,#14660,#14661,#14662,#14663,
#14664,#14665,#14666,#14667,#14668,#14669,#14670,#14671,#14672,#14673,#14674,
#14675,#14676),.UNSPECIFIED.,.F.,.F.,(4,2,2,2,2,2,2,2,4),(0.377311571006283,
0.47163860729283,0.565965643579376,0.660294392795971,0.754623142012565,
0.84895189122916,0.943280640445755,1.0376076767323,1.13193471301885),
 .UNSPECIFIED.);
#464=B_SPLINE_CURVE_WITH_KNOTS('',3,(#14677,#14678,#14679,#14680,#14681,
#14682,#14683,#14684,#14685,#14686),.UNSPECIFIED.,.F.,.F.,(4,2,2,2,4),(1.50924628402513,
1.60357503324173,1.69790378245832,1.79223081874487,1.88655785503141),
 .UNSPECIFIED.);
#465=B_SPLINE_CURVE_WITH_KNOTS('',3,(#14695,#14696,#14697,#14698,#14699,
#14700,#14701,#14702,#14703,#14704,#14705,#14706,#14707,#14708,#14709,#14710,
#14711,#14712),.UNSPECIFIED.,.F.,.F.,(4,2,2,2,2,2,2,2,4),(0.377311571006282,
0.471638607292829,0.565965643579376,0.660294392795971,0.754623142012565,
0.84895189122916,0.943280640445754,1.0376076767323,1.13193471301885),
 .UNSPECIFIED.);
#466=B_SPLINE_CURVE_WITH_KNOTS('',3,(#14714,#14715,#14716,#14717,#14718,
#14719,#14720,#14721,#14722,#14723),.UNSPECIFIED.,.F.,.F.,(4,2,2,2,4),(1.13193471301885,
1.22626174930539,1.32058878559194,1.41491753480854,1.50924628402513),
 .UNSPECIFIED.);
#467=B_SPLINE_CURVE_WITH_KNOTS('',3,(#14724,#14725,#14726,#14727,#14728,
#14729,#14730,#14731,#14732,#14733),.UNSPECIFIED.,.F.,.F.,(4,2,2,2,4),(1.50924628402513,
1.60357503324172,1.69790378245832,1.79223081874487,1.88655785503141),
 .UNSPECIFIED.);
#468=B_SPLINE_CURVE_WITH_KNOTS('',3,(#14736,#14737,#14738,#14739,#14740,
#14741,#14742,#14743,#14744,#14745,#14746,#14747,#14748,#14749,#14750,#14751,
#14752,#14753),.UNSPECIFIED.,.F.,.F.,(4,2,2,2,2,2,2,2,4),(0.377311571006283,
0.47163860729283,0.565965643579376,0.660294392795971,0.754623142012565,
0.84895189122916,0.943280640445754,1.0376076767323,1.13193471301885),
 .UNSPECIFIED.);
#469=B_SPLINE_CURVE_WITH_KNOTS('',3,(#14755,#14756,#14757,#14758,#14759,
#14760,#14761,#14762,#14763,#14764),.UNSPECIFIED.,.F.,.F.,(4,2,2,2,4),(1.13193471301885,
1.22626174930539,1.32058878559194,1.41491753480854,1.50924628402513),
 .UNSPECIFIED.);
#470=B_SPLINE_CURVE_WITH_KNOTS('',3,(#14765,#14766,#14767,#14768,#14769,
#14770,#14771,#14772,#14773,#14774),.UNSPECIFIED.,.F.,.F.,(4,2,2,2,4),(1.50924628402513,
1.60357503324173,1.69790378245832,1.79223081874487,1.88655785503141),
 .UNSPECIFIED.);
#471=B_SPLINE_CURVE_WITH_KNOTS('',3,(#14777,#14778,#14779,#14780,#14781,
#14782,#14783,#14784,#14785,#14786,#14787,#14788,#14789,#14790,#14791,#14792,
#14793,#14794),.UNSPECIFIED.,.F.,.F.,(4,2,2,2,2,2,2,2,4),(0.377311571006282,
0.471638607292829,0.565965643579376,0.66029439279597,0.754623142012565,
0.84895189122916,0.943280640445754,1.0376076767323,1.13193471301885),
 .UNSPECIFIED.);
#472=B_SPLINE_CURVE_WITH_KNOTS('',3,(#14796,#14797,#14798,#14799,#14800,
#14801,#14802,#14803,#14804,#14805),.UNSPECIFIED.,.F.,.F.,(4,2,2,2,4),(1.13193471301885,
1.22626174930539,1.32058878559194,1.41491753480854,1.50924628402513),
 .UNSPECIFIED.);
#473=B_SPLINE_CURVE_WITH_KNOTS('',3,(#14806,#14807,#14808,#14809,#14810,
#14811,#14812,#14813,#14814,#14815),.UNSPECIFIED.,.F.,.F.,(4,2,2,2,4),(1.50924628402513,
1.60357503324172,1.69790378245832,1.79223081874487,1.88655785503141),
 .UNSPECIFIED.);
#474=B_SPLINE_CURVE_WITH_KNOTS('',3,(#14818,#14819,#14820,#14821,#14822,
#14823,#14824,#14825,#14826,#14827,#14828,#14829,#14830,#14831,#14832,#14833,
#14834,#14835),.UNSPECIFIED.,.F.,.F.,(4,2,2,2,2,2,2,2,4),(0.377311571006283,
0.471638607292829,0.565965643579376,0.660294392795971,0.754623142012565,
0.84895189122916,0.943280640445755,1.0376076767323,1.13193471301885),
 .UNSPECIFIED.);
#475=B_SPLINE_CURVE_WITH_KNOTS('',3,(#14837,#14838,#14839,#14840,#14841,
#14842,#14843,#14844,#14845,#14846),.UNSPECIFIED.,.F.,.F.,(4,2,2,2,4),(1.13193471301885,
1.22626174930539,1.32058878559194,1.41491753480854,1.50924628402513),
 .UNSPECIFIED.);
#476=B_SPLINE_CURVE_WITH_KNOTS('',3,(#14847,#14848,#14849,#14850,#14851,
#14852,#14853,#14854,#14855,#14856),.UNSPECIFIED.,.F.,.F.,(4,2,2,2,4),(1.50924628402513,
1.60357503324172,1.69790378245832,1.79223081874487,1.88655785503141),
 .UNSPECIFIED.);
#477=B_SPLINE_CURVE_WITH_KNOTS('',3,(#14860,#14861,#14862,#14863,#14864,
#14865,#14866,#14867,#14868,#14869,#14870,#14871,#14872,#14873,#14874,#14875,
#14876,#14877,#14878,#14879,#14880,#14881,#14882,#14883,#14884,#14885,#14886,
#14887,#14888,#14889,#14890,#14891,#14892,#14893),.UNSPECIFIED.,.T.,.F.,
(4,2,2,2,2,2,2,2,2,2,2,2,2,2,2,2,4),(0.,0.0946120580087934,0.189224116017587,
0.283822945575014,0.378421775132442,0.47302060468987,0.567619434247297,
0.66223149225609,0.756843550264884,0.851455608273677,0.94606766628247,1.0406664958399,
1.13526532539733,1.22986415495475,1.32446298451218,1.41907504252097,1.51368710052977),
 .UNSPECIFIED.);
#478=B_SPLINE_CURVE_WITH_KNOTS('',3,(#14896,#14897,#14898,#14899,#14900,
#14901,#14902,#14903,#14904,#14905,#14906,#14907,#14908,#14909,#14910,#14911,
#14912,#14913,#14914,#14915,#14916,#14917,#14918,#14919,#14920,#14921,#14922,
#14923,#14924,#14925,#14926,#14927,#14928,#14929),.UNSPECIFIED.,.T.,.F.,
(4,2,2,2,2,2,2,2,2,2,2,2,2,2,2,2,4),(0.,0.0946120580087934,0.189224116017587,
0.283822945575014,0.378421775132442,0.47302060468987,0.567619434247297,
0.66223149225609,0.756843550264884,0.851455608273677,0.94606766628247,1.0406664958399,
1.13526532539733,1.22986415495475,1.32446298451218,1.41907504252097,1.51368710052977),
 .UNSPECIFIED.);
#479=B_SPLINE_CURVE_WITH_KNOTS('',3,(#14934,#14935,#14936,#14937,#14938,
#14939,#14940,#14941,#14942,#14943,#14944,#14945,#14946,#14947,#14948,#14949,
#14950,#14951,#14952,#14953,#14954,#14955,#14956,#14957,#14958,#14959,#14960,
#14961,#14962,#14963,#14964,#14965,#14966,#14967),.UNSPECIFIED.,.T.,.F.,
(4,2,2,2,2,2,2,2,2,2,2,2,2,2,2,2,4),(0.,0.0946120580087934,0.189224116017587,
0.283822945575014,0.378421775132442,0.47302060468987,0.567619434247297,
0.66223149225609,0.756843550264884,0.851455608273677,0.94606766628247,1.0406664958399,
1.13526532539733,1.22986415495475,1.32446298451218,1.41907504252097,1.51368710052977),
 .UNSPECIFIED.);
#480=B_SPLINE_CURVE_WITH_KNOTS('',3,(#14970,#14971,#14972,#14973,#14974,
#14975,#14976,#14977,#14978,#14979,#14980,#14981,#14982,#14983,#14984,#14985,
#14986,#14987,#14988,#14989,#14990,#14991,#14992,#14993,#14994,#14995,#14996,
#14997,#14998,#14999,#15000,#15001,#15002,#15003),.UNSPECIFIED.,.T.,.F.,
(4,2,2,2,2,2,2,2,2,2,2,2,2,2,2,2,4),(0.,0.0946120580087934,0.189224116017587,
0.283822945575014,0.378421775132442,0.47302060468987,0.567619434247297,
0.66223149225609,0.756843550264884,0.851455608273677,0.94606766628247,1.0406664958399,
1.13526532539733,1.22986415495475,1.32446298451218,1.41907504252097,1.51368710052977),
 .UNSPECIFIED.);
#481=B_SPLINE_CURVE_WITH_KNOTS('',3,(#15442,#15443,#15444,#15445,#15446,
#15447,#15448,#15449,#15450,#15451,#15452,#15453,#15454,#15455),
 .UNSPECIFIED.,.F.,.F.,(4,2,2,2,2,2,4),(0.756005737987026,0.793568827564645,
0.8729225200542,0.952276212543755,1.03162990503331,1.11098359752287,1.14854668710048),
 .UNSPECIFIED.);
#482=B_SPLINE_CURVE_WITH_KNOTS('',3,(#15461,#15462,#15463,#15464,#15465,
#15466,#15467,#15468,#15469,#15470,#15471,#15472,#15473,#15474,#15475,#15476,
#15477,#15478),.UNSPECIFIED.,.F.,.F.,(4,2,2,2,2,2,2,2,4),(0.,0.0792165807733624,
0.158433161546725,0.23764869707457,0.316864232602414,0.396079768130259,
0.475295303658103,0.554511884431466,0.633728465204828),.UNSPECIFIED.);
#483=B_SPLINE_CURVE_WITH_KNOTS('',3,(#15479,#15480,#15481,#15482,#15483,
#15484,#15485,#15486,#15487,#15488,#15489,#15490,#15491,#15492,#15493,#15494,
#15495,#15496),.UNSPECIFIED.,.F.,.F.,(4,2,2,2,2,2,2,2,4),(0.633728465204828,
0.712945045978191,0.792161626751553,0.871377162279398,0.950592697807242,
1.02980823333509,1.10902376886293,1.18824034963629,1.26745693040966),
 .UNSPECIFIED.);
#484=B_SPLINE_CURVE_WITH_KNOTS('',3,(#15499,#15500,#15501,#15502,#15503,
#15504,#15505,#15506,#15507,#15508,#15509,#15510,#15511,#15512),
 .UNSPECIFIED.,.F.,.F.,(4,2,2,2,2,2,4),(0.121154929624522,0.158718019202141,
0.238071711691697,0.317425404181252,0.396779096670807,0.476132789160362,
0.513695878737981),.UNSPECIFIED.);
#485=B_SPLINE_CURVE_WITH_KNOTS('',3,(#15537,#15538,#15539,#15540,#15541,
#15542,#15543,#15544,#15545,#15546,#15547,#15548,#15549,#15550),
 .UNSPECIFIED.,.F.,.F.,(4,2,2,2,2,2,4),(0.756005737987028,0.793568827564648,
0.872922520054202,0.952276212543757,1.03162990503331,1.11098359752287,1.14854668710049),
 .UNSPECIFIED.);
#486=B_SPLINE_CURVE_WITH_KNOTS('',3,(#15556,#15557,#15558,#15559,#15560,
#15561,#15562,#15563,#15564,#15565,#15566,#15567,#15568,#15569,#15570,#15571,
#15572,#15573),.UNSPECIFIED.,.F.,.F.,(4,2,2,2,2,2,2,2,4),(0.,0.0792165807733633,
0.158433161546727,0.237648697074571,0.316864232602415,0.396079768130259,
0.475295303658103,0.554511884431466,0.63372846520483),.UNSPECIFIED.);
#487=B_SPLINE_CURVE_WITH_KNOTS('',3,(#15574,#15575,#15576,#15577,#15578,
#15579,#15580,#15581,#15582,#15583,#15584,#15585,#15586,#15587,#15588,#15589,
#15590,#15591),.UNSPECIFIED.,.F.,.F.,(4,2,2,2,2,2,2,2,4),(0.63372846520483,
0.712945045978193,0.792161626751556,0.8713771622794,0.950592697807245,1.02980823333509,
1.10902376886293,1.1882403496363,1.26745693040966),.UNSPECIFIED.);
#488=B_SPLINE_CURVE_WITH_KNOTS('',3,(#15594,#15595,#15596,#15597,#15598,
#15599,#15600,#15601,#15602,#15603,#15604,#15605,#15606,#15607),
 .UNSPECIFIED.,.F.,.F.,(4,2,2,2,2,2,4),(0.121154929624524,0.158718019202143,
0.238071711691698,0.317425404181252,0.396779096670807,0.476132789160362,
0.513695878737981),.UNSPECIFIED.);
#489=B_SPLINE_CURVE_WITH_KNOTS('',3,(#15673,#15674,#15675,#15676,#15677,
#15678,#15679,#15680,#15681,#15682),.UNSPECIFIED.,.F.,.F.,(4,2,2,2,4),(0.168950313426779,
0.238079516586307,0.317435737633656,0.396791958681006,0.465921161840534),
 .UNSPECIFIED.);
#490=B_SPLINE_CURVE_WITH_KNOTS('',3,(#15686,#15687,#15688,#15689,#15690,
#15691),.UNSPECIFIED.,.F.,.F.,(4,2,4),(1.01510699658258,1.03166343394832,
1.10079263710785),.UNSPECIFIED.);
#491=B_SPLINE_CURVE_WITH_KNOTS('',3,(#15695,#15696,#15697,#15698,#15699,
#15700,#15701,#15702,#15703,#15704,#15705,#15706,#15707,#15708,#15709,#15710,
#15711,#15712,#15713,#15714,#15715,#15716,#15717,#15718,#15719,#15720,#15721,
#15722,#15723,#15724,#15725,#15726,#15727,#15728,#15729),.UNSPECIFIED.,
 .F.,.F.,(4,2,2,2,2,2,2,2,2,2,2,2,3,2,2,2,4),(0.379554434981269,0.396011596624156,
0.475213593758045,0.554416396369289,0.633619198980533,0.712822001591777,
0.792024804203021,0.87122680133691,0.950428798470799,1.02963079560469,1.10883279273858,
1.18803559534982,1.26723839796107,1.34644120057231,1.42564400318355,1.50484600031744,
1.52130316196033),.UNSPECIFIED.);
#492=B_SPLINE_CURVE_WITH_KNOTS('',3,(#15732,#15733,#15734,#15735,#15736,
#15737),.UNSPECIFIED.,.F.,.F.,(4,2,4),(0.803821788694091,0.872950991853619,
0.889507429219361),.UNSPECIFIED.);
#493=B_SPLINE_CURVE_WITH_KNOTS('',3,(#16156,#16157,#16158,#16159,#16160,
#16161,#16162,#16163,#16164,#16165,#16166,#16167,#16168,#16169,#16170,#16171,
#16172,#16173,#16174,#16175,#16176,#16177),.UNSPECIFIED.,.F.,.F.,(4,2,2,
2,2,2,2,2,2,2,4),(0.0473477652366656,0.126350602536658,0.189525903804987,
0.252701205073317,0.313298422430275,0.373895639787233,0.434492857144191,
0.495090074501149,0.558265375769478,0.621440677037807,0.7004435143378),
 .UNSPECIFIED.);
#494=B_SPLINE_CURVE_WITH_KNOTS('',3,(#16181,#16182,#16183,#16184,#16185,
#16186,#16187,#16188,#16189,#16190,#16191,#16192,#16193,#16194,#16195,#16196,
#16197,#16198,#16199,#16200,#16201,#16202),.UNSPECIFIED.,.F.,.F.,(4,2,2,
2,2,2,2,2,2,2,4),(0.0464897534940957,0.0852567806515119,0.170513561303024,
0.246687263103517,0.308657850341199,0.370628437578881,0.432599024816563,
0.494569612054245,0.570743313854739,0.656000094506251,0.694767121663666),
 .UNSPECIFIED.);
#495=B_SPLINE_CURVE_WITH_KNOTS('',3,(#16208,#16209,#16210,#16211,#16212,
#16213,#16214,#16215,#16216,#16217,#16218,#16219,#16220,#16221,#16222,#16223,
#16224,#16225,#16226,#16227,#16228,#16229),.UNSPECIFIED.,.F.,.F.,(4,2,2,
2,2,2,2,2,2,2,4),(0.0464897534940957,0.0852567806515118,0.170513561303024,
0.246687263103517,0.308657850341199,0.370628437578881,0.432599024816563,
0.494569612054245,0.570743313854738,0.65600009450625,0.694767121663666),
 .UNSPECIFIED.);
#496=B_SPLINE_CURVE_WITH_KNOTS('',3,(#16233,#16234,#16235,#16236,#16237,
#16238,#16239,#16240,#16241,#16242,#16243,#16244,#16245,#16246,#16247,#16248,
#16249,#16250,#16251,#16252,#16253,#16254),.UNSPECIFIED.,.F.,.F.,(4,2,2,
2,2,2,2,2,2,2,4),(0.0464897534940957,0.0852567806515119,0.170513561303024,
0.246687263103517,0.308657850341199,0.370628437578881,0.432599024816563,
0.494569612054245,0.570743313854739,0.656000094506251,0.694767121663666),
 .UNSPECIFIED.);
#497=B_SPLINE_CURVE_WITH_KNOTS('',3,(#16258,#16259,#16260,#16261,#16262,
#16263,#16264,#16265,#16266,#16267,#16268,#16269),.UNSPECIFIED.,.F.,.F.,
(4,2,2,2,2,4),(0.0464897534940957,0.0852567806515119,0.170513561303024,
0.246687263103517,0.308657850341199,0.370628437578881),.UNSPECIFIED.);
#498=B_SPLINE_CURVE_WITH_KNOTS('',3,(#16274,#16275,#16276,#16277,#16278,
#16279,#16280,#16281,#16282,#16283,#16284,#16285),.UNSPECIFIED.,.F.,.F.,
(4,2,2,2,2,4),(0.370628437578881,0.432599024816563,0.494569612054245,0.570743313854738,
0.65600009450625,0.694767121663666),.UNSPECIFIED.);
#499=B_SPLINE_CURVE_WITH_KNOTS('',3,(#16289,#16290,#16291,#16292,#16293,
#16294,#16295,#16296,#16297,#16298,#16299,#16300,#16301,#16302,#16303,#16304,
#16305,#16306,#16307,#16308,#16309,#16310),.UNSPECIFIED.,.F.,.F.,(4,2,2,
2,2,2,2,2,2,2,4),(0.0464897534940957,0.0852567806515121,0.170513561303024,
0.246687263103518,0.308657850341199,0.370628437578881,0.432599024816563,
0.494569612054245,0.570743313854738,0.65600009450625,0.694767121663666),
 .UNSPECIFIED.);
#500=B_SPLINE_CURVE_WITH_KNOTS('',3,(#16314,#16315,#16316,#16317,#16318,
#16319,#16320,#16321,#16322,#16323,#16324,#16325,#16326,#16327,#16328,#16329,
#16330,#16331,#16332,#16333,#16334,#16335),.UNSPECIFIED.,.F.,.F.,(4,2,2,
2,2,2,2,2,2,2,4),(0.0464897534940957,0.0852567806515119,0.170513561303024,
0.246687263103517,0.308657850341199,0.370628437578881,0.432599024816563,
0.494569612054245,0.570743313854738,0.65600009450625,0.694767121663667),
 .UNSPECIFIED.);
#501=B_SPLINE_CURVE_WITH_KNOTS('',3,(#16339,#16340,#16341,#16342,#16343,
#16344,#16345,#16346,#16347,#16348,#16349,#16350,#16351,#16352,#16353,#16354,
#16355,#16356,#16357,#16358,#16359,#16360),.UNSPECIFIED.,.F.,.F.,(4,2,2,
2,2,2,2,2,2,2,4),(0.0464897534940957,0.0852567806515119,0.170513561303024,
0.246687263103517,0.308657850341199,0.370628437578881,0.432599024816563,
0.494569612054245,0.570743313854738,0.65600009450625,0.694767121663666),
 .UNSPECIFIED.);
#502=B_SPLINE_CURVE_WITH_KNOTS('',3,(#16364,#16365,#16366,#16367,#16368,
#16369,#16370,#16371,#16372,#16373,#16374,#16375,#16376,#16377,#16378,#16379,
#16380,#16381,#16382,#16383,#16384,#16385),.UNSPECIFIED.,.F.,.F.,(4,2,2,
2,2,2,2,2,2,2,4),(0.0464897534940957,0.0852567806515119,0.170513561303024,
0.246687263103517,0.308657850341199,0.370628437578881,0.432599024816563,
0.494569612054245,0.570743313854739,0.656000094506251,0.694767121663667),
 .UNSPECIFIED.);
#503=B_SPLINE_CURVE_WITH_KNOTS('',3,(#16393,#16394,#16395,#16396,#16397,
#16398,#16399,#16400,#16401,#16402,#16403,#16404,#16405,#16406,#16407,#16408,
#16409,#16410,#16411,#16412,#16413,#16414),.UNSPECIFIED.,.F.,.F.,(4,2,2,
2,2,2,2,2,2,2,4),(0.0473477652366656,0.126350602536658,0.189525903804987,
0.252701205073316,0.313298422430274,0.373895639787232,0.434492857144191,
0.495090074501149,0.558265375769478,0.621440677037807,0.7004435143378),
 .UNSPECIFIED.);
#504=B_SPLINE_CURVE_WITH_KNOTS('',3,(#16422,#16423,#16424,#16425,#16426,
#16427,#16428,#16429,#16430,#16431,#16432,#16433,#16434,#16435,#16436,#16437,
#16438,#16439,#16440,#16441,#16442,#16443),.UNSPECIFIED.,.F.,.F.,(4,2,2,
2,2,2,2,2,2,2,4),(0.0473477652366656,0.126350602536658,0.189525903804987,
0.252701205073317,0.313298422430275,0.373895639787233,0.434492857144191,
0.495090074501149,0.558265375769478,0.621440677037807,0.7004435143378),
 .UNSPECIFIED.);
#505=B_SPLINE_CURVE_WITH_KNOTS('',3,(#16452,#16453,#16454,#16455,#16456,
#16457,#16458,#16459,#16460,#16461,#16462,#16463),.UNSPECIFIED.,.F.,.F.,
(4,2,2,2,2,4),(0.0473477652366656,0.126350602536658,0.189525903804987,0.252701205073316,
0.313298422430275,0.373895639787233),.UNSPECIFIED.);
#506=B_SPLINE_CURVE_WITH_KNOTS('',3,(#16465,#16466,#16467,#16468,#16469,
#16470,#16471,#16472,#16473,#16474,#16475,#16476),.UNSPECIFIED.,.F.,.F.,
(4,2,2,2,2,4),(0.373895639787233,0.434492857144191,0.495090074501149,0.558265375769478,
0.621440677037807,0.7004435143378),.UNSPECIFIED.);
#507=B_SPLINE_CURVE_WITH_KNOTS('',3,(#16483,#16484,#16485,#16486,#16487,
#16488,#16489,#16490,#16491,#16492,#16493,#16494,#16495,#16496,#16497,#16498,
#16499,#16500,#16501,#16502,#16503,#16504),.UNSPECIFIED.,.F.,.F.,(4,2,2,
2,2,2,2,2,2,2,4),(0.0473477652366656,0.126350602536658,0.189525903804987,
0.252701205073316,0.313298422430275,0.373895639787233,0.434492857144191,
0.495090074501149,0.558265375769478,0.621440677037807,0.7004435143378),
 .UNSPECIFIED.);
#508=B_SPLINE_CURVE_WITH_KNOTS('',3,(#16512,#16513,#16514,#16515,#16516,
#16517,#16518,#16519,#16520,#16521,#16522,#16523,#16524,#16525,#16526,#16527,
#16528,#16529,#16530,#16531,#16532,#16533),.UNSPECIFIED.,.F.,.F.,(4,2,2,
2,2,2,2,2,2,2,4),(0.0473477652366656,0.126350602536658,0.189525903804987,
0.252701205073317,0.313298422430275,0.373895639787233,0.434492857144191,
0.495090074501149,0.558265375769478,0.621440677037807,0.7004435143378),
 .UNSPECIFIED.);
#509=B_SPLINE_CURVE_WITH_KNOTS('',3,(#16541,#16542,#16543,#16544,#16545,
#16546,#16547,#16548,#16549,#16550,#16551,#16552,#16553,#16554,#16555,#16556,
#16557,#16558,#16559,#16560,#16561,#16562),.UNSPECIFIED.,.F.,.F.,(4,2,2,
2,2,2,2,2,2,2,4),(0.0473477652366656,0.126350602536658,0.189525903804987,
0.252701205073316,0.313298422430275,0.373895639787233,0.434492857144191,
0.495090074501149,0.558265375769478,0.621440677037807,0.7004435143378),
 .UNSPECIFIED.);
#510=B_SPLINE_CURVE_WITH_KNOTS('',3,(#16571,#16572,#16573,#16574,#16575,
#16576,#16577,#16578,#16579,#16580,#16581,#16582,#16583,#16584,#16585,#16586,
#16587,#16588,#16589,#16590,#16591,#16592),.UNSPECIFIED.,.F.,.F.,(4,2,2,
2,2,2,2,2,2,2,4),(0.0473477652366656,0.126350602536658,0.189525903804987,
0.252701205073317,0.313298422430275,0.373895639787233,0.434492857144191,
0.495090074501149,0.558265375769478,0.621440677037807,0.7004435143378),
 .UNSPECIFIED.);
#511=SPHERICAL_SURFACE('',#9980,2.35);
#512=SPHERICAL_SURFACE('',#10020,2.35);
#513=SPHERICAL_SURFACE('',#10435,0.23815);
#514=SPHERICAL_SURFACE('',#10437,0.23815);
#515=SPHERICAL_SURFACE('',#10439,0.23815);
#516=SPHERICAL_SURFACE('',#10441,0.23815);
#517=SPHERICAL_SURFACE('',#10443,0.23815);
#518=SPHERICAL_SURFACE('',#10445,0.23815);
#519=SPHERICAL_SURFACE('',#10447,0.23815);
#520=SPHERICAL_SURFACE('',#10449,0.23815);
#521=SPHERICAL_SURFACE('',#10452,0.247676);
#522=SPHERICAL_SURFACE('',#10468,0.247676);
#523=SPHERICAL_SURFACE('',#10473,0.247676);
#524=SPHERICAL_SURFACE('',#10478,0.247676);
#525=SPHERICAL_SURFACE('',#10483,0.247676);
#526=SPHERICAL_SURFACE('',#10488,0.247676);
#527=SPHERICAL_SURFACE('',#10493,0.247676);
#528=SPHERICAL_SURFACE('',#10501,0.247676);
#529=ORIENTED_CLOSED_SHELL('',*,#9058,.F.);
#530=ORIENTED_CLOSED_SHELL('',*,#9063,.F.);
#531=ORIENTED_CLOSED_SHELL('',*,#9067,.F.);
#532=ORIENTED_CLOSED_SHELL('',*,#9070,.F.);
#533=ORIENTED_CLOSED_SHELL('',*,#9110,.F.);
#534=CONICAL_SURFACE('',#9949,0.4,0.785398163397448);
#535=CONICAL_SURFACE('',#9953,0.41,0.785398163397448);
#536=CONICAL_SURFACE('',#9957,0.26,0.463647609000806);
#537=CONICAL_SURFACE('',#9961,0.225,0.785398163397448);
#538=CONICAL_SURFACE('',#10066,0.625,0.785398163397448);
#539=CONICAL_SURFACE('',#10070,0.635,0.785398163397449);
#540=CONICAL_SURFACE('',#10074,0.41,0.463647609000806);
#541=CONICAL_SURFACE('',#10116,0.275,0.785398163397449);
#542=CONICAL_SURFACE('',#10139,0.4,0.785398163397448);
#543=CONICAL_SURFACE('',#10143,0.41,0.785398163397448);
#544=CONICAL_SURFACE('',#10147,0.26,0.463647609000806);
#545=CONICAL_SURFACE('',#10153,0.325,0.785398163397448);
#546=CONICAL_SURFACE('',#10157,0.335,0.785398163397448);
#547=CONICAL_SURFACE('',#10161,0.21,0.463647609000806);
#548=CONICAL_SURFACE('',#10165,0.18,0.785398163397448);
#549=CONICAL_SURFACE('',#10179,0.55,0.785398163397448);
#550=CONICAL_SURFACE('',#10332,0.235,0.785398163397448);
#551=CONICAL_SURFACE('',#10336,0.2125,0.785398163397448);
#552=CONICAL_SURFACE('',#10406,0.53,0.785398163397448);
#553=CONICAL_SURFACE('',#10413,0.53,0.785398163397448);
#554=CONICAL_SURFACE('',#10426,1.47,0.785398163397449);
#555=CONICAL_SURFACE('',#10430,1.47,0.785398163397449);
#556=CONICAL_SURFACE('',#10724,0.325,0.785398163397448);
#557=CONICAL_SURFACE('',#10728,0.335,0.785398163397448);
#558=CONICAL_SURFACE('',#10732,0.21,0.463647609000806);
#559=BREP_WITH_VOIDS('Body1',#9057,(#529));
#560=BREP_WITH_VOIDS('Body1',#9064,(#530));
#561=BREP_WITH_VOIDS('Body1',#9068,(#531));
#562=BREP_WITH_VOIDS('Body1',#9069,(#532));
#563=BREP_WITH_VOIDS('Body1',#9111,(#533));
#564=SHAPE_REPRESENTATION_RELATIONSHIP('SRR','None',#17560,#616);
#565=SHAPE_REPRESENTATION_RELATIONSHIP('SRR','None',#17561,#617);
#566=SHAPE_REPRESENTATION_RELATIONSHIP('SRR','None',#17562,#618);
#567=SHAPE_REPRESENTATION_RELATIONSHIP('SRR','None',#17563,#619);
#568=SHAPE_REPRESENTATION_RELATIONSHIP('SRR','None',#17564,#620);
#569=SHAPE_REPRESENTATION_RELATIONSHIP('SRR','None',#17565,#621);
#570=SHAPE_REPRESENTATION_RELATIONSHIP('SRR','None',#17566,#622);
#571=SHAPE_REPRESENTATION_RELATIONSHIP('SRR','None',#17567,#623);
#572=SHAPE_REPRESENTATION_RELATIONSHIP('SRR','None',#17568,#624);
#573=SHAPE_REPRESENTATION_RELATIONSHIP('SRR','None',#17569,#625);
#574=SHAPE_REPRESENTATION_RELATIONSHIP('SRR','None',#17570,#626);
#575=SHAPE_REPRESENTATION_RELATIONSHIP('SRR','None',#17571,#627);
#576=SHAPE_REPRESENTATION_RELATIONSHIP('SRR','None',#17573,#628);
#577=SHAPE_REPRESENTATION_RELATIONSHIP('SRR','None',#17574,#629);
#578=SHAPE_REPRESENTATION_RELATIONSHIP('SRR','None',#17575,#630);
#579=SHAPE_REPRESENTATION_RELATIONSHIP('SRR','None',#17576,#631);
#580=SHAPE_REPRESENTATION_RELATIONSHIP('SRR','None',#17577,#632);
#581=SHAPE_REPRESENTATION_RELATIONSHIP('SRR','None',#17578,#633);
#582=SHAPE_REPRESENTATION_RELATIONSHIP('SRR','None',#17579,#634);
#583=SHAPE_REPRESENTATION_RELATIONSHIP('SRR','None',#17580,#635);
#584=SHAPE_REPRESENTATION_RELATIONSHIP('SRR','None',#17581,#636);
#585=SHAPE_REPRESENTATION_RELATIONSHIP('SRR','None',#17583,#637);
#586=SHAPE_REPRESENTATION_RELATIONSHIP('SRR','None',#17584,#638);
#587=SHAPE_REPRESENTATION_RELATIONSHIP('SRR','None',#17585,#639);
#588=SHAPE_REPRESENTATION_RELATIONSHIP('SRR','None',#17586,#640);
#589=SHAPE_REPRESENTATION_RELATIONSHIP('SRR','None',#17587,#641);
#590=SHAPE_REPRESENTATION_RELATIONSHIP('SRR','None',#17588,#642);
#591=SHAPE_REPRESENTATION_RELATIONSHIP('SRR','None',#17589,#643);
#592=SHAPE_REPRESENTATION_RELATIONSHIP('SRR','None',#17590,#644);
#593=SHAPE_REPRESENTATION_RELATIONSHIP('SRR','None',#17591,#645);
#594=SHAPE_REPRESENTATION_RELATIONSHIP('SRR','None',#17592,#646);
#595=SHAPE_REPRESENTATION_RELATIONSHIP('SRR','None',#17593,#647);
#596=SHAPE_REPRESENTATION_RELATIONSHIP('SRR','None',#17595,#648);
#597=SHAPE_REPRESENTATION_RELATIONSHIP('SRR','None',#17596,#649);
#598=SHAPE_REPRESENTATION_RELATIONSHIP('SRR','None',#17597,#650);
#599=SHAPE_REPRESENTATION_RELATIONSHIP('SRR','None',#17598,#651);
#600=SHAPE_REPRESENTATION_RELATIONSHIP('SRR','None',#17599,#652);
#601=SHAPE_REPRESENTATION_RELATIONSHIP('SRR','None',#17601,#653);
#602=SHAPE_REPRESENTATION_RELATIONSHIP('SRR','None',#17602,#654);
#603=SHAPE_REPRESENTATION_RELATIONSHIP('SRR','None',#17603,#655);
#604=SHAPE_REPRESENTATION_RELATIONSHIP('SRR','None',#17604,#656);
#605=SHAPE_REPRESENTATION_RELATIONSHIP('SRR','None',#17605,#657);
#606=SHAPE_REPRESENTATION_RELATIONSHIP('SRR','None',#17607,#658);
#607=SHAPE_REPRESENTATION_RELATIONSHIP('SRR','None',#17608,#659);
#608=SHAPE_REPRESENTATION_RELATIONSHIP('SRR','None',#17609,#660);
#609=SHAPE_REPRESENTATION_RELATIONSHIP('SRR','None',#17610,#661);
#610=SHAPE_REPRESENTATION_RELATIONSHIP('SRR','None',#17611,#662);
#611=SHAPE_REPRESENTATION_RELATIONSHIP('SRR','None',#17612,#663);
#612=SHAPE_REPRESENTATION_RELATIONSHIP('SRR','None',#17613,#664);
#613=SHAPE_REPRESENTATION_RELATIONSHIP('SRR','None',#17615,#665);
#614=SHAPE_REPRESENTATION_RELATIONSHIP('SRR','None',#17616,#666);
#615=SHAPE_REPRESENTATION_RELATIONSHIP('SRR','None',#17617,#667);
#616=ADVANCED_BREP_SHAPE_REPRESENTATION('',(#729),#17264);
#617=ADVANCED_BREP_SHAPE_REPRESENTATION('',(#730),#17265);
#618=ADVANCED_BREP_SHAPE_REPRESENTATION('',(#731),#17266);
#619=ADVANCED_BREP_SHAPE_REPRESENTATION('',(#732),#17267);
#620=ADVANCED_BREP_SHAPE_REPRESENTATION('',(#733),#17268);
#621=ADVANCED_BREP_SHAPE_REPRESENTATION('',(#734),#17269);
#622=ADVANCED_BREP_SHAPE_REPRESENTATION('',(#735),#17270);
#623=ADVANCED_BREP_SHAPE_REPRESENTATION('',(#736),#17271);
#624=ADVANCED_BREP_SHAPE_REPRESENTATION('',(#737),#17272);
#625=ADVANCED_BREP_SHAPE_REPRESENTATION('',(#738),#17273);
#626=ADVANCED_BREP_SHAPE_REPRESENTATION('',(#739),#17274);
#627=ADVANCED_BREP_SHAPE_REPRESENTATION('',(#559),#17275);
#628=ADVANCED_BREP_SHAPE_REPRESENTATION('',(#740),#17277);
#629=ADVANCED_BREP_SHAPE_REPRESENTATION('',(#741,#742),#17278);
#630=ADVANCED_BREP_SHAPE_REPRESENTATION('',(#743),#17279);
#631=ADVANCED_BREP_SHAPE_REPRESENTATION('',(#560),#17280);
#632=ADVANCED_BREP_SHAPE_REPRESENTATION('',(#744),#17281);
#633=ADVANCED_BREP_SHAPE_REPRESENTATION('',(#745),#17282);
#634=ADVANCED_BREP_SHAPE_REPRESENTATION('',(#561),#17283);
#635=ADVANCED_BREP_SHAPE_REPRESENTATION('',(#562),#17284);
#636=ADVANCED_BREP_SHAPE_REPRESENTATION('',(#746),#17285);
#637=ADVANCED_BREP_SHAPE_REPRESENTATION('',(#747),#17287);
#638=ADVANCED_BREP_SHAPE_REPRESENTATION('',(#748),#17288);
#639=ADVANCED_BREP_SHAPE_REPRESENTATION('',(#749),#17289);
#640=ADVANCED_BREP_SHAPE_REPRESENTATION('',(#750),#17290);
#641=ADVANCED_BREP_SHAPE_REPRESENTATION('',(#751),#17291);
#642=ADVANCED_BREP_SHAPE_REPRESENTATION('',(#752),#17292);
#643=ADVANCED_BREP_SHAPE_REPRESENTATION('',(#753),#17293);
#644=ADVANCED_BREP_SHAPE_REPRESENTATION('',(#754),#17294);
#645=ADVANCED_BREP_SHAPE_REPRESENTATION('',(#755),#17295);
#646=ADVANCED_BREP_SHAPE_REPRESENTATION('',(#756),#17296);
#647=ADVANCED_BREP_SHAPE_REPRESENTATION('',(#757),#17297);
#648=ADVANCED_BREP_SHAPE_REPRESENTATION('',(#758),#17299);
#649=ADVANCED_BREP_SHAPE_REPRESENTATION('',(#759),#17300);
#650=ADVANCED_BREP_SHAPE_REPRESENTATION('',(#760),#17301);
#651=ADVANCED_BREP_SHAPE_REPRESENTATION('',(#761),#17302);
#652=ADVANCED_BREP_SHAPE_REPRESENTATION('',(#762),#17303);
#653=ADVANCED_BREP_SHAPE_REPRESENTATION('',(#763),#17305);
#654=ADVANCED_BREP_SHAPE_REPRESENTATION('',(#764),#17306);
#655=ADVANCED_BREP_SHAPE_REPRESENTATION('',(#765,#766,#767,#768,#769,#770,
#771,#772),#17307);
#656=ADVANCED_BREP_SHAPE_REPRESENTATION('',(#773),#17308);
#657=ADVANCED_BREP_SHAPE_REPRESENTATION('',(#774,#775),#17309);
#658=ADVANCED_BREP_SHAPE_REPRESENTATION('',(#776),#17311);
#659=ADVANCED_BREP_SHAPE_REPRESENTATION('',(#777),#17312);
#660=ADVANCED_BREP_SHAPE_REPRESENTATION('',(#778),#17313);
#661=ADVANCED_BREP_SHAPE_REPRESENTATION('',(#779),#17314);
#662=ADVANCED_BREP_SHAPE_REPRESENTATION('',(#780),#17315);
#663=ADVANCED_BREP_SHAPE_REPRESENTATION('',(#781),#17316);
#664=ADVANCED_BREP_SHAPE_REPRESENTATION('',(#782),#17317);
#665=ADVANCED_BREP_SHAPE_REPRESENTATION('',(#783),#17319);
#666=ADVANCED_BREP_SHAPE_REPRESENTATION('',(#784),#17320);
#667=ADVANCED_BREP_SHAPE_REPRESENTATION('',(#563),#17321);
#668=STYLED_ITEM('',(#17910),#729);
#669=STYLED_ITEM('',(#17931),#730);
#670=STYLED_ITEM('',(#17938),#731);
#671=STYLED_ITEM('',(#17938),#732);
#672=STYLED_ITEM('',(#17931),#733);
#673=STYLED_ITEM('',(#17938),#734);
#674=STYLED_ITEM('',(#17938),#735);
#675=STYLED_ITEM('',(#17945),#736);
#676=STYLED_ITEM('',(#17945),#737);
#677=STYLED_ITEM('',(#17917),#738);
#678=STYLED_ITEM('',(#17917),#739);
#679=STYLED_ITEM('',(#17938),#559);
#680=STYLED_ITEM('',(#17910),#740);
#681=STYLED_ITEM('',(#17931),#741);
#682=STYLED_ITEM('',(#17931),#742);
#683=STYLED_ITEM('',(#17938),#743);
#684=STYLED_ITEM('',(#17938),#560);
#685=STYLED_ITEM('',(#17931),#744);
#686=STYLED_ITEM('',(#17938),#745);
#687=STYLED_ITEM('',(#17938),#561);
#688=STYLED_ITEM('',(#17938),#562);
#689=STYLED_ITEM('',(#17931),#746);
#690=STYLED_ITEM('',(#17931),#747);
#691=STYLED_ITEM('',(#17931),#748);
#692=STYLED_ITEM('',(#17931),#749);
#693=STYLED_ITEM('',(#17931),#750);
#694=STYLED_ITEM('',(#17945),#751);
#695=STYLED_ITEM('',(#17931),#752);
#696=STYLED_ITEM('',(#17931),#753);
#697=STYLED_ITEM('',(#17931),#754);
#698=STYLED_ITEM('',(#17931),#755);
#699=STYLED_ITEM('',(#17931),#756);
#700=STYLED_ITEM('',(#17938),#757);
#701=STYLED_ITEM('',(#17931),#758);
#702=STYLED_ITEM('',(#17931),#759);
#703=STYLED_ITEM('',(#17931),#760);
#704=STYLED_ITEM('',(#17931),#761);
#705=STYLED_ITEM('',(#17931),#762);
#706=STYLED_ITEM('',(#17931),#763);
#707=STYLED_ITEM('',(#17931),#764);
#708=STYLED_ITEM('',(#17931),#765);
#709=STYLED_ITEM('',(#17931),#766);
#710=STYLED_ITEM('',(#17931),#767);
#711=STYLED_ITEM('',(#17931),#768);
#712=STYLED_ITEM('',(#17931),#769);
#713=STYLED_ITEM('',(#17931),#770);
#714=STYLED_ITEM('',(#17931),#771);
#715=STYLED_ITEM('',(#17931),#772);
#716=STYLED_ITEM('',(#17931),#773);
#717=STYLED_ITEM('',(#17931),#774);
#718=STYLED_ITEM('',(#17931),#775);
#719=STYLED_ITEM('',(#17910),#776);
#720=STYLED_ITEM('',(#17924),#777);
#721=STYLED_ITEM('',(#17924),#778);
#722=STYLED_ITEM('',(#17931),#779);
#723=STYLED_ITEM('',(#17931),#780);
#724=STYLED_ITEM('',(#17931),#781);
#725=STYLED_ITEM('',(#17931),#782);
#726=STYLED_ITEM('',(#17945),#783);
#727=STYLED_ITEM('',(#17924),#784);
#728=STYLED_ITEM('',(#17938),#563);
#729=MANIFOLD_SOLID_BREP('Body1',#9046);
#730=MANIFOLD_SOLID_BREP('Body1',#9047);
#731=MANIFOLD_SOLID_BREP('Body1',#9048);
#732=MANIFOLD_SOLID_BREP('Body1',#9049);
#733=MANIFOLD_SOLID_BREP('Body1',#9050);
#734=MANIFOLD_SOLID_BREP('Body1',#9051);
#735=MANIFOLD_SOLID_BREP('Body1',#9052);
#736=MANIFOLD_SOLID_BREP('Body1',#9053);
#737=MANIFOLD_SOLID_BREP('Body1',#9054);
#738=MANIFOLD_SOLID_BREP('Body1',#9055);
#739=MANIFOLD_SOLID_BREP('Body1',#9056);
#740=MANIFOLD_SOLID_BREP('Body1',#9059);
#741=MANIFOLD_SOLID_BREP('Body1',#9060);
#742=MANIFOLD_SOLID_BREP('Body2',#9061);
#743=MANIFOLD_SOLID_BREP('Body1',#9062);
#744=MANIFOLD_SOLID_BREP('Body1',#9065);
#745=MANIFOLD_SOLID_BREP('Body1',#9066);
#746=MANIFOLD_SOLID_BREP('Body1',#9071);
#747=MANIFOLD_SOLID_BREP('Body1',#9072);
#748=MANIFOLD_SOLID_BREP('Body1',#9073);
#749=MANIFOLD_SOLID_BREP('Body1',#9074);
#750=MANIFOLD_SOLID_BREP('Body1',#9075);
#751=MANIFOLD_SOLID_BREP('Body1',#9076);
#752=MANIFOLD_SOLID_BREP('Body1',#9077);
#753=MANIFOLD_SOLID_BREP('Body1',#9078);
#754=MANIFOLD_SOLID_BREP('Body1',#9079);
#755=MANIFOLD_SOLID_BREP('Body1',#9080);
#756=MANIFOLD_SOLID_BREP('Body1',#9081);
#757=MANIFOLD_SOLID_BREP('Body1',#9082);
#758=MANIFOLD_SOLID_BREP('Body1',#9083);
#759=MANIFOLD_SOLID_BREP('Body1',#9084);
#760=MANIFOLD_SOLID_BREP('Body1',#9085);
#761=MANIFOLD_SOLID_BREP('Body1',#9086);
#762=MANIFOLD_SOLID_BREP('Body1',#9087);
#763=MANIFOLD_SOLID_BREP('Body1',#9088);
#764=MANIFOLD_SOLID_BREP('Body1',#9089);
#765=MANIFOLD_SOLID_BREP('Body1',#9090);
#766=MANIFOLD_SOLID_BREP('Body2',#9091);
#767=MANIFOLD_SOLID_BREP('Body3',#9092);
#768=MANIFOLD_SOLID_BREP('Body4',#9093);
#769=MANIFOLD_SOLID_BREP('Body5',#9094);
#770=MANIFOLD_SOLID_BREP('Body6',#9095);
#771=MANIFOLD_SOLID_BREP('Body7',#9096);
#772=MANIFOLD_SOLID_BREP('Body8',#9097);
#773=MANIFOLD_SOLID_BREP('Continuous crown cage',#9098);
#774=MANIFOLD_SOLID_BREP('Body1',#9099);
#775=MANIFOLD_SOLID_BREP('Body2',#9100);
#776=MANIFOLD_SOLID_BREP('Body1',#9101);
#777=MANIFOLD_SOLID_BREP('Body1',#9102);
#778=MANIFOLD_SOLID_BREP('Body1',#9103);
#779=MANIFOLD_SOLID_BREP('Body1',#9104);
#780=MANIFOLD_SOLID_BREP('Body1',#9105);
#781=MANIFOLD_SOLID_BREP('Body1',#9106);
#782=MANIFOLD_SOLID_BREP('Body1',#9107);
#783=MANIFOLD_SOLID_BREP('Body1',#9108);
#784=MANIFOLD_SOLID_BREP('Body1',#9109);
#785=FACE_BOUND('',#1872,.T.);
#786=FACE_BOUND('',#1873,.T.);
#787=FACE_BOUND('',#1874,.T.);
#788=FACE_BOUND('',#1875,.T.);
#789=FACE_BOUND('',#1876,.T.);
#790=FACE_BOUND('',#1877,.T.);
#791=FACE_BOUND('',#1878,.T.);
#792=FACE_BOUND('',#1879,.T.);
#793=FACE_BOUND('',#1880,.T.);
#794=FACE_BOUND('',#1881,.T.);
#795=FACE_BOUND('',#1882,.T.);
#796=FACE_BOUND('',#1883,.T.);
#797=FACE_BOUND('',#1885,.T.);
#798=FACE_BOUND('',#1886,.T.);
#799=FACE_BOUND('',#1887,.T.);
#800=FACE_BOUND('',#1888,.T.);
#801=FACE_BOUND('',#1889,.T.);
#802=FACE_BOUND('',#1890,.T.);
#803=FACE_BOUND('',#1891,.T.);
#804=FACE_BOUND('',#1892,.T.);
#805=FACE_BOUND('',#1893,.T.);
#806=FACE_BOUND('',#1894,.T.);
#807=FACE_BOUND('',#1895,.T.);
#808=FACE_BOUND('',#1896,.T.);
#809=FACE_BOUND('',#1903,.T.);
#810=FACE_BOUND('',#1906,.T.);
#811=FACE_BOUND('',#1909,.T.);
#812=FACE_BOUND('',#1912,.T.);
#813=FACE_BOUND('',#1922,.T.);
#814=FACE_BOUND('',#1923,.T.);
#815=FACE_BOUND('',#1924,.T.);
#816=FACE_BOUND('',#1925,.T.);
#817=FACE_BOUND('',#1926,.T.);
#818=FACE_BOUND('',#1927,.T.);
#819=FACE_BOUND('',#1929,.T.);
#820=FACE_BOUND('',#1930,.T.);
#821=FACE_BOUND('',#1931,.T.);
#822=FACE_BOUND('',#1932,.T.);
#823=FACE_BOUND('',#1936,.T.);
#824=FACE_BOUND('',#1938,.T.);
#825=FACE_BOUND('',#1942,.T.);
#826=FACE_BOUND('',#1944,.T.);
#827=FACE_BOUND('',#1951,.T.);
#828=FACE_BOUND('',#1954,.T.);
#829=FACE_BOUND('',#1957,.T.);
#830=FACE_BOUND('',#1960,.T.);
#831=FACE_BOUND('',#1970,.T.);
#832=FACE_BOUND('',#1971,.T.);
#833=FACE_BOUND('',#1972,.T.);
#834=FACE_BOUND('',#1973,.T.);
#835=FACE_BOUND('',#1974,.T.);
#836=FACE_BOUND('',#1975,.T.);
#837=FACE_BOUND('',#1977,.T.);
#838=FACE_BOUND('',#1978,.T.);
#839=FACE_BOUND('',#1979,.T.);
#840=FACE_BOUND('',#1980,.T.);
#841=FACE_BOUND('',#1984,.T.);
#842=FACE_BOUND('',#1986,.T.);
#843=FACE_BOUND('',#1990,.T.);
#844=FACE_BOUND('',#1992,.T.);
#845=FACE_BOUND('',#1996,.T.);
#846=FACE_BOUND('',#1999,.T.);
#847=FACE_BOUND('',#2001,.T.);
#848=FACE_BOUND('',#2002,.T.);
#849=FACE_BOUND('',#2003,.T.);
#850=FACE_BOUND('',#2004,.T.);
#851=FACE_BOUND('',#2020,.T.);
#852=FACE_BOUND('',#2021,.T.);
#853=FACE_BOUND('',#2025,.T.);
#854=FACE_BOUND('',#2028,.T.);
#855=FACE_BOUND('',#2030,.T.);
#856=FACE_BOUND('',#2031,.T.);
#857=FACE_BOUND('',#2032,.T.);
#858=FACE_BOUND('',#2033,.T.);
#859=FACE_BOUND('',#2049,.T.);
#860=FACE_BOUND('',#2050,.T.);
#861=FACE_BOUND('',#2068,.T.);
#862=FACE_BOUND('',#2084,.T.);
#863=FACE_BOUND('',#2085,.T.);
#864=FACE_BOUND('',#2093,.T.);
#865=FACE_BOUND('',#2094,.T.);
#866=FACE_BOUND('',#2095,.T.);
#867=FACE_BOUND('',#2098,.T.);
#868=FACE_BOUND('',#2100,.T.);
#869=FACE_BOUND('',#2113,.T.);
#870=FACE_BOUND('',#2114,.T.);
#871=FACE_BOUND('',#2115,.T.);
#872=FACE_BOUND('',#2118,.T.);
#873=FACE_BOUND('',#2120,.T.);
#874=FACE_BOUND('',#2121,.T.);
#875=FACE_BOUND('',#2123,.T.);
#876=FACE_BOUND('',#2127,.T.);
#877=FACE_BOUND('',#2128,.T.);
#878=FACE_BOUND('',#2129,.T.);
#879=FACE_BOUND('',#2130,.T.);
#880=FACE_BOUND('',#2131,.T.);
#881=FACE_BOUND('',#2132,.T.);
#882=FACE_BOUND('',#2138,.T.);
#883=FACE_BOUND('',#2140,.T.);
#884=FACE_BOUND('',#2143,.T.);
#885=FACE_BOUND('',#2145,.T.);
#886=FACE_BOUND('',#2146,.T.);
#887=FACE_BOUND('',#2147,.T.);
#888=FACE_BOUND('',#2148,.T.);
#889=FACE_BOUND('',#2149,.T.);
#890=FACE_BOUND('',#2150,.T.);
#891=FACE_BOUND('',#2154,.T.);
#892=FACE_BOUND('',#2156,.T.);
#893=FACE_BOUND('',#2171,.T.);
#894=FACE_BOUND('',#2179,.T.);
#895=FACE_BOUND('',#2181,.T.);
#896=FACE_BOUND('',#2183,.T.);
#897=FACE_BOUND('',#2190,.T.);
#898=FACE_BOUND('',#2193,.T.);
#899=FACE_BOUND('',#2194,.T.);
#900=FACE_BOUND('',#2197,.T.);
#901=FACE_BOUND('',#2200,.T.);
#902=FACE_BOUND('',#2203,.T.);
#903=FACE_BOUND('',#2206,.T.);
#904=FACE_BOUND('',#2210,.T.);
#905=FACE_BOUND('',#2213,.T.);
#906=FACE_BOUND('',#2228,.T.);
#907=FACE_BOUND('',#2236,.T.);
#908=FACE_BOUND('',#2264,.T.);
#909=FACE_BOUND('',#2266,.T.);
#910=FACE_BOUND('',#2268,.T.);
#911=FACE_BOUND('',#2270,.T.);
#912=FACE_BOUND('',#2275,.T.);
#913=FACE_BOUND('',#2277,.T.);
#914=FACE_BOUND('',#2279,.T.);
#915=FACE_BOUND('',#2281,.T.);
#916=FACE_BOUND('',#2285,.T.);
#917=FACE_BOUND('',#2287,.T.);
#918=FACE_BOUND('',#2290,.T.);
#919=FACE_BOUND('',#2301,.T.);
#920=FACE_BOUND('',#2302,.T.);
#921=FACE_BOUND('',#2304,.T.);
#922=FACE_BOUND('',#2312,.T.);
#923=FACE_BOUND('',#2315,.T.);
#924=FACE_BOUND('',#2321,.T.);
#925=FACE_BOUND('',#2323,.T.);
#926=FACE_BOUND('',#2327,.T.);
#927=FACE_BOUND('',#2329,.T.);
#928=FACE_BOUND('',#2333,.T.);
#929=FACE_BOUND('',#2335,.T.);
#930=FACE_BOUND('',#2354,.T.);
#931=FACE_BOUND('',#2363,.T.);
#932=FACE_BOUND('',#2364,.T.);
#933=FACE_BOUND('',#2369,.T.);
#934=FACE_BOUND('',#2370,.T.);
#935=FACE_BOUND('',#2374,.T.);
#936=FACE_BOUND('',#2376,.T.);
#937=FACE_BOUND('',#2380,.T.);
#938=FACE_BOUND('',#2382,.T.);
#939=FACE_BOUND('',#2386,.T.);
#940=FACE_BOUND('',#2388,.T.);
#941=FACE_BOUND('',#2392,.T.);
#942=FACE_BOUND('',#2394,.T.);
#943=FACE_BOUND('',#2400,.T.);
#944=FACE_BOUND('',#2403,.T.);
#945=FACE_BOUND('',#2408,.T.);
#946=FACE_BOUND('',#2413,.T.);
#947=FACE_BOUND('',#2441,.T.);
#948=FACE_BOUND('',#2444,.T.);
#949=FACE_BOUND('',#2447,.T.);
#950=FACE_BOUND('',#2450,.T.);
#951=FACE_BOUND('',#2453,.T.);
#952=FACE_BOUND('',#2457,.T.);
#953=FACE_BOUND('',#2462,.T.);
#954=FACE_BOUND('',#2471,.T.);
#955=FACE_BOUND('',#2472,.T.);
#956=FACE_BOUND('',#2473,.T.);
#957=FACE_BOUND('',#2474,.T.);
#958=FACE_BOUND('',#2475,.T.);
#959=FACE_BOUND('',#2476,.T.);
#960=FACE_BOUND('',#2479,.T.);
#961=FACE_BOUND('',#2480,.T.);
#962=FACE_BOUND('',#2481,.T.);
#963=FACE_BOUND('',#2482,.T.);
#964=FACE_BOUND('',#2483,.T.);
#965=FACE_BOUND('',#2484,.T.);
#966=FACE_BOUND('',#2486,.T.);
#967=FACE_BOUND('',#2496,.T.);
#968=FACE_BOUND('',#2497,.T.);
#969=FACE_BOUND('',#2498,.T.);
#970=FACE_BOUND('',#2499,.T.);
#971=FACE_BOUND('',#2500,.T.);
#972=FACE_BOUND('',#2501,.T.);
#973=FACE_BOUND('',#2504,.T.);
#974=FACE_BOUND('',#2505,.T.);
#975=FACE_BOUND('',#2506,.T.);
#976=FACE_BOUND('',#2507,.T.);
#977=FACE_BOUND('',#2508,.T.);
#978=FACE_BOUND('',#2509,.T.);
#979=FACE_BOUND('',#2520,.T.);
#980=FACE_BOUND('',#2521,.T.);
#981=FACE_BOUND('',#2522,.T.);
#982=FACE_BOUND('',#2523,.T.);
#983=FACE_BOUND('',#2524,.T.);
#984=FACE_BOUND('',#2525,.T.);
#985=FACE_BOUND('',#2528,.T.);
#986=FACE_BOUND('',#2529,.T.);
#987=FACE_BOUND('',#2530,.T.);
#988=FACE_BOUND('',#2531,.T.);
#989=FACE_BOUND('',#2532,.T.);
#990=FACE_BOUND('',#2533,.T.);
#991=FACE_BOUND('',#2539,.T.);
#992=FACE_BOUND('',#2544,.T.);
#993=FACE_BOUND('',#2548,.T.);
#994=FACE_BOUND('',#2550,.T.);
#995=FACE_BOUND('',#2554,.T.);
#996=FACE_BOUND('',#2556,.T.);
#997=FACE_BOUND('',#2560,.T.);
#998=FACE_BOUND('',#2562,.T.);
#999=FACE_BOUND('',#2569,.T.);
#1000=FACE_BOUND('',#2572,.T.);
#1001=FACE_BOUND('',#2575,.T.);
#1002=FACE_BOUND('',#2578,.T.);
#1003=FACE_BOUND('',#2581,.T.);
#1004=FACE_BOUND('',#2584,.T.);
#1005=FACE_BOUND('',#2586,.T.);
#1006=FACE_BOUND('',#2592,.T.);
#1007=FACE_BOUND('',#2594,.T.);
#1008=FACE_BOUND('',#2596,.T.);
#1009=FACE_BOUND('',#2598,.T.);
#1010=FACE_BOUND('',#2613,.T.);
#1011=PLANE('',#9724);
#1012=PLANE('',#9725);
#1013=PLANE('',#9726);
#1014=PLANE('',#9727);
#1015=PLANE('',#9728);
#1016=PLANE('',#9729);
#1017=PLANE('',#9734);
#1018=PLANE('',#9738);
#1019=PLANE('',#9742);
#1020=PLANE('',#9747);
#1021=PLANE('',#9752);
#1022=PLANE('',#9757);
#1023=PLANE('',#9767);
#1024=PLANE('',#9768);
#1025=PLANE('',#9769);
#1026=PLANE('',#9770);
#1027=PLANE('',#9771);
#1028=PLANE('',#9772);
#1029=PLANE('',#9780);
#1030=PLANE('',#9781);
#1031=PLANE('',#9789);
#1032=PLANE('',#9790);
#1033=PLANE('',#9795);
#1034=PLANE('',#9799);
#1035=PLANE('',#9803);
#1036=PLANE('',#9808);
#1037=PLANE('',#9813);
#1038=PLANE('',#9818);
#1039=PLANE('',#9828);
#1040=PLANE('',#9829);
#1041=PLANE('',#9830);
#1042=PLANE('',#9831);
#1043=PLANE('',#9832);
#1044=PLANE('',#9833);
#1045=PLANE('',#9841);
#1046=PLANE('',#9842);
#1047=PLANE('',#9850);
#1048=PLANE('',#9851);
#1049=PLANE('',#9859);
#1050=PLANE('',#9864);
#1051=PLANE('',#9866);
#1052=PLANE('',#9877);
#1053=PLANE('',#9880);
#1054=PLANE('',#9883);
#1055=PLANE('',#9886);
#1056=PLANE('',#9887);
#1057=PLANE('',#9888);
#1058=PLANE('',#9889);
#1059=PLANE('',#9890);
#1060=PLANE('',#9891);
#1061=PLANE('',#9899);
#1062=PLANE('',#9904);
#1063=PLANE('',#9906);
#1064=PLANE('',#9917);
#1065=PLANE('',#9920);
#1066=PLANE('',#9923);
#1067=PLANE('',#9926);
#1068=PLANE('',#9927);
#1069=PLANE('',#9928);
#1070=PLANE('',#9929);
#1071=PLANE('',#9930);
#1072=PLANE('',#9931);
#1073=PLANE('',#9933);
#1074=PLANE('',#9934);
#1075=PLANE('',#9935);
#1076=PLANE('',#9936);
#1077=PLANE('',#9937);
#1078=PLANE('',#9938);
#1079=PLANE('',#9940);
#1080=PLANE('',#9941);
#1081=PLANE('',#9942);
#1082=PLANE('',#9943);
#1083=PLANE('',#9944);
#1084=PLANE('',#9945);
#1085=PLANE('',#9947);
#1086=PLANE('',#9955);
#1087=PLANE('',#9963);
#1088=PLANE('',#9964);
#1089=PLANE('',#9965);
#1090=PLANE('',#9966);
#1091=PLANE('',#9967);
#1092=PLANE('',#9968);
#1093=PLANE('',#9969);
#1094=PLANE('',#9970);
#1095=PLANE('',#9971);
#1096=PLANE('',#9982);
#1097=PLANE('',#9984);
#1098=PLANE('',#9986);
#1099=PLANE('',#9988);
#1100=PLANE('',#9989);
#1101=PLANE('',#9991);
#1102=PLANE('',#9992);
#1103=PLANE('',#9998);
#1104=PLANE('',#9999);
#1105=PLANE('',#10000);
#1106=PLANE('',#10001);
#1107=PLANE('',#10002);
#1108=PLANE('',#10003);
#1109=PLANE('',#10004);
#1110=PLANE('',#10009);
#1111=PLANE('',#10010);
#1112=PLANE('',#10011);
#1113=PLANE('',#10012);
#1114=PLANE('',#10013);
#1115=PLANE('',#10018);
#1116=PLANE('',#10023);
#1117=PLANE('',#10033);
#1118=PLANE('',#10035);
#1119=PLANE('',#10039);
#1120=PLANE('',#10051);
#1121=PLANE('',#10052);
#1122=PLANE('',#10054);
#1123=PLANE('',#10055);
#1124=PLANE('',#10056);
#1125=PLANE('',#10057);
#1126=PLANE('',#10058);
#1127=PLANE('',#10059);
#1128=PLANE('',#10060);
#1129=PLANE('',#10061);
#1130=PLANE('',#10062);
#1131=PLANE('',#10064);
#1132=PLANE('',#10072);
#1133=PLANE('',#10078);
#1134=PLANE('',#10085);
#1135=PLANE('',#10086);
#1136=PLANE('',#10088);
#1137=PLANE('',#10090);
#1138=PLANE('',#10104);
#1139=PLANE('',#10105);
#1140=PLANE('',#10106);
#1141=PLANE('',#10107);
#1142=PLANE('',#10108);
#1143=PLANE('',#10109);
#1144=PLANE('',#10110);
#1145=PLANE('',#10111);
#1146=PLANE('',#10112);
#1147=PLANE('',#10113);
#1148=PLANE('',#10114);
#1149=PLANE('',#10121);
#1150=PLANE('',#10125);
#1151=PLANE('',#10127);
#1152=PLANE('',#10128);
#1153=PLANE('',#10129);
#1154=PLANE('',#10130);
#1155=PLANE('',#10131);
#1156=PLANE('',#10132);
#1157=PLANE('',#10133);
#1158=PLANE('',#10134);
#1159=PLANE('',#10135);
#1160=PLANE('',#10137);
#1161=PLANE('',#10145);
#1162=PLANE('',#10151);
#1163=PLANE('',#10159);
#1164=PLANE('',#10167);
#1165=PLANE('',#10168);
#1166=PLANE('',#10169);
#1167=PLANE('',#10170);
#1168=PLANE('',#10171);
#1169=PLANE('',#10172);
#1170=PLANE('',#10173);
#1171=PLANE('',#10174);
#1172=PLANE('',#10175);
#1173=PLANE('',#10177);
#1174=PLANE('',#10183);
#1175=PLANE('',#10186);
#1176=PLANE('',#10187);
#1177=PLANE('',#10189);
#1178=PLANE('',#10190);
#1179=PLANE('',#10195);
#1180=PLANE('',#10196);
#1181=PLANE('',#10198);
#1182=PLANE('',#10203);
#1183=PLANE('',#10210);
#1184=PLANE('',#10211);
#1185=PLANE('',#10213);
#1186=PLANE('',#10218);
#1187=PLANE('',#10225);
#1188=PLANE('',#10226);
#1189=PLANE('',#10234);
#1190=PLANE('',#10235);
#1191=PLANE('',#10240);
#1192=PLANE('',#10246);
#1193=PLANE('',#10247);
#1194=PLANE('',#10251);
#1195=PLANE('',#10255);
#1196=PLANE('',#10256);
#1197=PLANE('',#10257);
#1198=PLANE('',#10258);
#1199=PLANE('',#10261);
#1200=PLANE('',#10269);
#1201=PLANE('',#10274);
#1202=PLANE('',#10275);
#1203=PLANE('',#10280);
#1204=PLANE('',#10283);
#1205=PLANE('',#10291);
#1206=PLANE('',#10292);
#1207=PLANE('',#10300);
#1208=PLANE('',#10301);
#1209=PLANE('',#10309);
#1210=PLANE('',#10310);
#1211=PLANE('',#10312);
#1212=PLANE('',#10313);
#1213=PLANE('',#10314);
#1214=PLANE('',#10315);
#1215=PLANE('',#10316);
#1216=PLANE('',#10317);
#1217=PLANE('',#10318);
#1218=PLANE('',#10319);
#1219=PLANE('',#10320);
#1220=PLANE('',#10321);
#1221=PLANE('',#10323);
#1222=PLANE('',#10324);
#1223=PLANE('',#10325);
#1224=PLANE('',#10326);
#1225=PLANE('',#10327);
#1226=PLANE('',#10328);
#1227=PLANE('',#10329);
#1228=PLANE('',#10330);
#1229=PLANE('',#10338);
#1230=PLANE('',#10350);
#1231=PLANE('',#10352);
#1232=PLANE('',#10355);
#1233=PLANE('',#10356);
#1234=PLANE('',#10364);
#1235=PLANE('',#10365);
#1236=PLANE('',#10373);
#1237=PLANE('',#10374);
#1238=PLANE('',#10382);
#1239=PLANE('',#10383);
#1240=PLANE('',#10391);
#1241=PLANE('',#10392);
#1242=PLANE('',#10408);
#1243=PLANE('',#10411);
#1244=PLANE('',#10423);
#1245=PLANE('',#10432);
#1246=PLANE('',#10465);
#1247=PLANE('',#10470);
#1248=PLANE('',#10475);
#1249=PLANE('',#10480);
#1250=PLANE('',#10485);
#1251=PLANE('',#10490);
#1252=PLANE('',#10499);
#1253=PLANE('',#10503);
#1254=PLANE('',#10504);
#1255=PLANE('',#10506);
#1256=PLANE('',#10511);
#1257=PLANE('',#10514);
#1258=PLANE('',#10519);
#1259=PLANE('',#10539);
#1260=PLANE('',#10540);
#1261=PLANE('',#10541);
#1262=PLANE('',#10542);
#1263=PLANE('',#10543);
#1264=PLANE('',#10562);
#1265=PLANE('',#10563);
#1266=PLANE('',#10564);
#1267=PLANE('',#10565);
#1268=PLANE('',#10566);
#1269=PLANE('',#10567);
#1270=PLANE('',#10587);
#1271=PLANE('',#10588);
#1272=PLANE('',#10589);
#1273=PLANE('',#10590);
#1274=PLANE('',#10591);
#1275=PLANE('',#10592);
#1276=PLANE('',#10612);
#1277=PLANE('',#10613);
#1278=PLANE('',#10614);
#1279=PLANE('',#10615);
#1280=PLANE('',#10616);
#1281=PLANE('',#10617);
#1282=PLANE('',#10622);
#1283=PLANE('',#10623);
#1284=PLANE('',#10628);
#1285=PLANE('',#10631);
#1286=PLANE('',#10639);
#1287=PLANE('',#10640);
#1288=PLANE('',#10648);
#1289=PLANE('',#10649);
#1290=PLANE('',#10657);
#1291=PLANE('',#10658);
#1292=PLANE('',#10661);
#1293=PLANE('',#10663);
#1294=PLANE('',#10664);
#1295=PLANE('',#10666);
#1296=PLANE('',#10667);
#1297=PLANE('',#10668);
#1298=PLANE('',#10673);
#1299=PLANE('',#10677);
#1300=PLANE('',#10681);
#1301=PLANE('',#10685);
#1302=PLANE('',#10689);
#1303=PLANE('',#10693);
#1304=PLANE('',#10696);
#1305=PLANE('',#10697);
#1306=PLANE('',#10700);
#1307=PLANE('',#10701);
#1308=PLANE('',#10706);
#1309=PLANE('',#10712);
#1310=PLANE('',#10713);
#1311=PLANE('',#10714);
#1312=PLANE('',#10715);
#1313=PLANE('',#10716);
#1314=PLANE('',#10717);
#1315=PLANE('',#10718);
#1316=PLANE('',#10719);
#1317=PLANE('',#10720);
#1318=PLANE('',#10722);
#1319=PLANE('',#10730);
#1320=FACE_OUTER_BOUND('',#1855,.T.);
#1321=FACE_OUTER_BOUND('',#1856,.T.);
#1322=FACE_OUTER_BOUND('',#1857,.T.);
#1323=FACE_OUTER_BOUND('',#1858,.T.);
#1324=FACE_OUTER_BOUND('',#1859,.T.);
#1325=FACE_OUTER_BOUND('',#1860,.T.);
#1326=FACE_OUTER_BOUND('',#1861,.T.);
#1327=FACE_OUTER_BOUND('',#1862,.T.);
#1328=FACE_OUTER_BOUND('',#1863,.T.);
#1329=FACE_OUTER_BOUND('',#1864,.T.);
#1330=FACE_OUTER_BOUND('',#1865,.T.);
#1331=FACE_OUTER_BOUND('',#1866,.T.);
#1332=FACE_OUTER_BOUND('',#1867,.T.);
#1333=FACE_OUTER_BOUND('',#1868,.T.);
#1334=FACE_OUTER_BOUND('',#1869,.T.);
#1335=FACE_OUTER_BOUND('',#1870,.T.);
#1336=FACE_OUTER_BOUND('',#1871,.T.);
#1337=FACE_OUTER_BOUND('',#1884,.T.);
#1338=FACE_OUTER_BOUND('',#1897,.T.);
#1339=FACE_OUTER_BOUND('',#1898,.T.);
#1340=FACE_OUTER_BOUND('',#1899,.T.);
#1341=FACE_OUTER_BOUND('',#1900,.T.);
#1342=FACE_OUTER_BOUND('',#1901,.T.);
#1343=FACE_OUTER_BOUND('',#1902,.T.);
#1344=FACE_OUTER_BOUND('',#1904,.T.);
#1345=FACE_OUTER_BOUND('',#1905,.T.);
#1346=FACE_OUTER_BOUND('',#1907,.T.);
#1347=FACE_OUTER_BOUND('',#1908,.T.);
#1348=FACE_OUTER_BOUND('',#1910,.T.);
#1349=FACE_OUTER_BOUND('',#1911,.T.);
#1350=FACE_OUTER_BOUND('',#1913,.T.);
#1351=FACE_OUTER_BOUND('',#1914,.T.);
#1352=FACE_OUTER_BOUND('',#1915,.T.);
#1353=FACE_OUTER_BOUND('',#1916,.T.);
#1354=FACE_OUTER_BOUND('',#1917,.T.);
#1355=FACE_OUTER_BOUND('',#1918,.T.);
#1356=FACE_OUTER_BOUND('',#1919,.T.);
#1357=FACE_OUTER_BOUND('',#1920,.T.);
#1358=FACE_OUTER_BOUND('',#1921,.T.);
#1359=FACE_OUTER_BOUND('',#1928,.T.);
#1360=FACE_OUTER_BOUND('',#1933,.T.);
#1361=FACE_OUTER_BOUND('',#1934,.T.);
#1362=FACE_OUTER_BOUND('',#1935,.T.);
#1363=FACE_OUTER_BOUND('',#1937,.T.);
#1364=FACE_OUTER_BOUND('',#1939,.T.);
#1365=FACE_OUTER_BOUND('',#1940,.T.);
#1366=FACE_OUTER_BOUND('',#1941,.T.);
#1367=FACE_OUTER_BOUND('',#1943,.T.);
#1368=FACE_OUTER_BOUND('',#1945,.T.);
#1369=FACE_OUTER_BOUND('',#1946,.T.);
#1370=FACE_OUTER_BOUND('',#1947,.T.);
#1371=FACE_OUTER_BOUND('',#1948,.T.);
#1372=FACE_OUTER_BOUND('',#1949,.T.);
#1373=FACE_OUTER_BOUND('',#1950,.T.);
#1374=FACE_OUTER_BOUND('',#1952,.T.);
#1375=FACE_OUTER_BOUND('',#1953,.T.);
#1376=FACE_OUTER_BOUND('',#1955,.T.);
#1377=FACE_OUTER_BOUND('',#1956,.T.);
#1378=FACE_OUTER_BOUND('',#1958,.T.);
#1379=FACE_OUTER_BOUND('',#1959,.T.);
#1380=FACE_OUTER_BOUND('',#1961,.T.);
#1381=FACE_OUTER_BOUND('',#1962,.T.);
#1382=FACE_OUTER_BOUND('',#1963,.T.);
#1383=FACE_OUTER_BOUND('',#1964,.T.);
#1384=FACE_OUTER_BOUND('',#1965,.T.);
#1385=FACE_OUTER_BOUND('',#1966,.T.);
#1386=FACE_OUTER_BOUND('',#1967,.T.);
#1387=FACE_OUTER_BOUND('',#1968,.T.);
#1388=FACE_OUTER_BOUND('',#1969,.T.);
#1389=FACE_OUTER_BOUND('',#1976,.T.);
#1390=FACE_OUTER_BOUND('',#1981,.T.);
#1391=FACE_OUTER_BOUND('',#1982,.T.);
#1392=FACE_OUTER_BOUND('',#1983,.T.);
#1393=FACE_OUTER_BOUND('',#1985,.T.);
#1394=FACE_OUTER_BOUND('',#1987,.T.);
#1395=FACE_OUTER_BOUND('',#1988,.T.);
#1396=FACE_OUTER_BOUND('',#1989,.T.);
#1397=FACE_OUTER_BOUND('',#1991,.T.);
#1398=FACE_OUTER_BOUND('',#1993,.T.);
#1399=FACE_OUTER_BOUND('',#1994,.T.);
#1400=FACE_OUTER_BOUND('',#1995,.T.);
#1401=FACE_OUTER_BOUND('',#1997,.T.);
#1402=FACE_OUTER_BOUND('',#1998,.T.);
#1403=FACE_OUTER_BOUND('',#2000,.T.);
#1404=FACE_OUTER_BOUND('',#2005,.T.);
#1405=FACE_OUTER_BOUND('',#2006,.T.);
#1406=FACE_OUTER_BOUND('',#2007,.T.);
#1407=FACE_OUTER_BOUND('',#2008,.T.);
#1408=FACE_OUTER_BOUND('',#2009,.T.);
#1409=FACE_OUTER_BOUND('',#2010,.T.);
#1410=FACE_OUTER_BOUND('',#2011,.T.);
#1411=FACE_OUTER_BOUND('',#2012,.T.);
#1412=FACE_OUTER_BOUND('',#2013,.T.);
#1413=FACE_OUTER_BOUND('',#2014,.T.);
#1414=FACE_OUTER_BOUND('',#2015,.T.);
#1415=FACE_OUTER_BOUND('',#2016,.T.);
#1416=FACE_OUTER_BOUND('',#2017,.T.);
#1417=FACE_OUTER_BOUND('',#2018,.T.);
#1418=FACE_OUTER_BOUND('',#2019,.T.);
#1419=FACE_OUTER_BOUND('',#2022,.T.);
#1420=FACE_OUTER_BOUND('',#2023,.T.);
#1421=FACE_OUTER_BOUND('',#2024,.T.);
#1422=FACE_OUTER_BOUND('',#2026,.T.);
#1423=FACE_OUTER_BOUND('',#2027,.T.);
#1424=FACE_OUTER_BOUND('',#2029,.T.);
#1425=FACE_OUTER_BOUND('',#2034,.T.);
#1426=FACE_OUTER_BOUND('',#2035,.T.);
#1427=FACE_OUTER_BOUND('',#2036,.T.);
#1428=FACE_OUTER_BOUND('',#2037,.T.);
#1429=FACE_OUTER_BOUND('',#2038,.T.);
#1430=FACE_OUTER_BOUND('',#2039,.T.);
#1431=FACE_OUTER_BOUND('',#2040,.T.);
#1432=FACE_OUTER_BOUND('',#2041,.T.);
#1433=FACE_OUTER_BOUND('',#2042,.T.);
#1434=FACE_OUTER_BOUND('',#2043,.T.);
#1435=FACE_OUTER_BOUND('',#2044,.T.);
#1436=FACE_OUTER_BOUND('',#2045,.T.);
#1437=FACE_OUTER_BOUND('',#2046,.T.);
#1438=FACE_OUTER_BOUND('',#2047,.T.);
#1439=FACE_OUTER_BOUND('',#2048,.T.);
#1440=FACE_OUTER_BOUND('',#2051,.T.);
#1441=FACE_OUTER_BOUND('',#2052,.T.);
#1442=FACE_OUTER_BOUND('',#2053,.T.);
#1443=FACE_OUTER_BOUND('',#2054,.T.);
#1444=FACE_OUTER_BOUND('',#2055,.T.);
#1445=FACE_OUTER_BOUND('',#2056,.T.);
#1446=FACE_OUTER_BOUND('',#2057,.T.);
#1447=FACE_OUTER_BOUND('',#2058,.T.);
#1448=FACE_OUTER_BOUND('',#2059,.T.);
#1449=FACE_OUTER_BOUND('',#2060,.T.);
#1450=FACE_OUTER_BOUND('',#2061,.T.);
#1451=FACE_OUTER_BOUND('',#2062,.T.);
#1452=FACE_OUTER_BOUND('',#2063,.T.);
#1453=FACE_OUTER_BOUND('',#2064,.T.);
#1454=FACE_OUTER_BOUND('',#2065,.T.);
#1455=FACE_OUTER_BOUND('',#2066,.T.);
#1456=FACE_OUTER_BOUND('',#2067,.T.);
#1457=FACE_OUTER_BOUND('',#2069,.T.);
#1458=FACE_OUTER_BOUND('',#2070,.T.);
#1459=FACE_OUTER_BOUND('',#2071,.T.);
#1460=FACE_OUTER_BOUND('',#2072,.T.);
#1461=FACE_OUTER_BOUND('',#2073,.T.);
#1462=FACE_OUTER_BOUND('',#2074,.T.);
#1463=FACE_OUTER_BOUND('',#2075,.T.);
#1464=FACE_OUTER_BOUND('',#2076,.T.);
#1465=FACE_OUTER_BOUND('',#2077,.T.);
#1466=FACE_OUTER_BOUND('',#2078,.T.);
#1467=FACE_OUTER_BOUND('',#2079,.T.);
#1468=FACE_OUTER_BOUND('',#2080,.T.);
#1469=FACE_OUTER_BOUND('',#2081,.T.);
#1470=FACE_OUTER_BOUND('',#2082,.T.);
#1471=FACE_OUTER_BOUND('',#2083,.T.);
#1472=FACE_OUTER_BOUND('',#2086,.T.);
#1473=FACE_OUTER_BOUND('',#2087,.T.);
#1474=FACE_OUTER_BOUND('',#2088,.T.);
#1475=FACE_OUTER_BOUND('',#2089,.T.);
#1476=FACE_OUTER_BOUND('',#2090,.T.);
#1477=FACE_OUTER_BOUND('',#2091,.T.);
#1478=FACE_OUTER_BOUND('',#2092,.T.);
#1479=FACE_OUTER_BOUND('',#2096,.T.);
#1480=FACE_OUTER_BOUND('',#2097,.T.);
#1481=FACE_OUTER_BOUND('',#2099,.T.);
#1482=FACE_OUTER_BOUND('',#2101,.T.);
#1483=FACE_OUTER_BOUND('',#2102,.T.);
#1484=FACE_OUTER_BOUND('',#2103,.T.);
#1485=FACE_OUTER_BOUND('',#2104,.T.);
#1486=FACE_OUTER_BOUND('',#2105,.T.);
#1487=FACE_OUTER_BOUND('',#2106,.T.);
#1488=FACE_OUTER_BOUND('',#2107,.T.);
#1489=FACE_OUTER_BOUND('',#2108,.T.);
#1490=FACE_OUTER_BOUND('',#2109,.T.);
#1491=FACE_OUTER_BOUND('',#2110,.T.);
#1492=FACE_OUTER_BOUND('',#2111,.T.);
#1493=FACE_OUTER_BOUND('',#2112,.T.);
#1494=FACE_OUTER_BOUND('',#2116,.T.);
#1495=FACE_OUTER_BOUND('',#2117,.T.);
#1496=FACE_OUTER_BOUND('',#2119,.T.);
#1497=FACE_OUTER_BOUND('',#2122,.T.);
#1498=FACE_OUTER_BOUND('',#2124,.T.);
#1499=FACE_OUTER_BOUND('',#2125,.T.);
#1500=FACE_OUTER_BOUND('',#2126,.T.);
#1501=FACE_OUTER_BOUND('',#2133,.T.);
#1502=FACE_OUTER_BOUND('',#2134,.T.);
#1503=FACE_OUTER_BOUND('',#2135,.T.);
#1504=FACE_OUTER_BOUND('',#2136,.T.);
#1505=FACE_OUTER_BOUND('',#2137,.T.);
#1506=FACE_OUTER_BOUND('',#2139,.T.);
#1507=FACE_OUTER_BOUND('',#2141,.T.);
#1508=FACE_OUTER_BOUND('',#2142,.T.);
#1509=FACE_OUTER_BOUND('',#2144,.T.);
#1510=FACE_OUTER_BOUND('',#2151,.T.);
#1511=FACE_OUTER_BOUND('',#2152,.T.);
#1512=FACE_OUTER_BOUND('',#2153,.T.);
#1513=FACE_OUTER_BOUND('',#2155,.T.);
#1514=FACE_OUTER_BOUND('',#2157,.T.);
#1515=FACE_OUTER_BOUND('',#2158,.T.);
#1516=FACE_OUTER_BOUND('',#2159,.T.);
#1517=FACE_OUTER_BOUND('',#2160,.T.);
#1518=FACE_OUTER_BOUND('',#2161,.T.);
#1519=FACE_OUTER_BOUND('',#2162,.T.);
#1520=FACE_OUTER_BOUND('',#2163,.T.);
#1521=FACE_OUTER_BOUND('',#2164,.T.);
#1522=FACE_OUTER_BOUND('',#2165,.T.);
#1523=FACE_OUTER_BOUND('',#2166,.T.);
#1524=FACE_OUTER_BOUND('',#2167,.T.);
#1525=FACE_OUTER_BOUND('',#2168,.T.);
#1526=FACE_OUTER_BOUND('',#2169,.T.);
#1527=FACE_OUTER_BOUND('',#2170,.T.);
#1528=FACE_OUTER_BOUND('',#2172,.T.);
#1529=FACE_OUTER_BOUND('',#2173,.T.);
#1530=FACE_OUTER_BOUND('',#2174,.T.);
#1531=FACE_OUTER_BOUND('',#2175,.T.);
#1532=FACE_OUTER_BOUND('',#2176,.T.);
#1533=FACE_OUTER_BOUND('',#2177,.T.);
#1534=FACE_OUTER_BOUND('',#2178,.T.);
#1535=FACE_OUTER_BOUND('',#2180,.T.);
#1536=FACE_OUTER_BOUND('',#2182,.T.);
#1537=FACE_OUTER_BOUND('',#2184,.T.);
#1538=FACE_OUTER_BOUND('',#2185,.T.);
#1539=FACE_OUTER_BOUND('',#2186,.T.);
#1540=FACE_OUTER_BOUND('',#2187,.T.);
#1541=FACE_OUTER_BOUND('',#2188,.T.);
#1542=FACE_OUTER_BOUND('',#2189,.T.);
#1543=FACE_OUTER_BOUND('',#2191,.T.);
#1544=FACE_OUTER_BOUND('',#2192,.T.);
#1545=FACE_OUTER_BOUND('',#2195,.T.);
#1546=FACE_OUTER_BOUND('',#2196,.T.);
#1547=FACE_OUTER_BOUND('',#2198,.T.);
#1548=FACE_OUTER_BOUND('',#2199,.T.);
#1549=FACE_OUTER_BOUND('',#2201,.T.);
#1550=FACE_OUTER_BOUND('',#2202,.T.);
#1551=FACE_OUTER_BOUND('',#2204,.T.);
#1552=FACE_OUTER_BOUND('',#2205,.T.);
#1553=FACE_OUTER_BOUND('',#2207,.T.);
#1554=FACE_OUTER_BOUND('',#2208,.T.);
#1555=FACE_OUTER_BOUND('',#2209,.T.);
#1556=FACE_OUTER_BOUND('',#2211,.T.);
#1557=FACE_OUTER_BOUND('',#2212,.T.);
#1558=FACE_OUTER_BOUND('',#2214,.T.);
#1559=FACE_OUTER_BOUND('',#2215,.T.);
#1560=FACE_OUTER_BOUND('',#2216,.T.);
#1561=FACE_OUTER_BOUND('',#2217,.T.);
#1562=FACE_OUTER_BOUND('',#2218,.T.);
#1563=FACE_OUTER_BOUND('',#2219,.T.);
#1564=FACE_OUTER_BOUND('',#2220,.T.);
#1565=FACE_OUTER_BOUND('',#2221,.T.);
#1566=FACE_OUTER_BOUND('',#2222,.T.);
#1567=FACE_OUTER_BOUND('',#2223,.T.);
#1568=FACE_OUTER_BOUND('',#2224,.T.);
#1569=FACE_OUTER_BOUND('',#2225,.T.);
#1570=FACE_OUTER_BOUND('',#2226,.T.);
#1571=FACE_OUTER_BOUND('',#2227,.T.);
#1572=FACE_OUTER_BOUND('',#2229,.T.);
#1573=FACE_OUTER_BOUND('',#2230,.T.);
#1574=FACE_OUTER_BOUND('',#2231,.T.);
#1575=FACE_OUTER_BOUND('',#2232,.T.);
#1576=FACE_OUTER_BOUND('',#2233,.T.);
#1577=FACE_OUTER_BOUND('',#2234,.T.);
#1578=FACE_OUTER_BOUND('',#2235,.T.);
#1579=FACE_OUTER_BOUND('',#2237,.T.);
#1580=FACE_OUTER_BOUND('',#2238,.T.);
#1581=FACE_OUTER_BOUND('',#2239,.T.);
#1582=FACE_OUTER_BOUND('',#2240,.T.);
#1583=FACE_OUTER_BOUND('',#2241,.T.);
#1584=FACE_OUTER_BOUND('',#2242,.T.);
#1585=FACE_OUTER_BOUND('',#2243,.T.);
#1586=FACE_OUTER_BOUND('',#2244,.T.);
#1587=FACE_OUTER_BOUND('',#2245,.T.);
#1588=FACE_OUTER_BOUND('',#2246,.T.);
#1589=FACE_OUTER_BOUND('',#2247,.T.);
#1590=FACE_OUTER_BOUND('',#2248,.T.);
#1591=FACE_OUTER_BOUND('',#2249,.T.);
#1592=FACE_OUTER_BOUND('',#2250,.T.);
#1593=FACE_OUTER_BOUND('',#2251,.T.);
#1594=FACE_OUTER_BOUND('',#2252,.T.);
#1595=FACE_OUTER_BOUND('',#2253,.T.);
#1596=FACE_OUTER_BOUND('',#2254,.T.);
#1597=FACE_OUTER_BOUND('',#2255,.T.);
#1598=FACE_OUTER_BOUND('',#2256,.T.);
#1599=FACE_OUTER_BOUND('',#2257,.T.);
#1600=FACE_OUTER_BOUND('',#2258,.T.);
#1601=FACE_OUTER_BOUND('',#2259,.T.);
#1602=FACE_OUTER_BOUND('',#2260,.T.);
#1603=FACE_OUTER_BOUND('',#2261,.T.);
#1604=FACE_OUTER_BOUND('',#2262,.T.);
#1605=FACE_OUTER_BOUND('',#2263,.T.);
#1606=FACE_OUTER_BOUND('',#2265,.T.);
#1607=FACE_OUTER_BOUND('',#2267,.T.);
#1608=FACE_OUTER_BOUND('',#2269,.T.);
#1609=FACE_OUTER_BOUND('',#2271,.T.);
#1610=FACE_OUTER_BOUND('',#2272,.T.);
#1611=FACE_OUTER_BOUND('',#2273,.T.);
#1612=FACE_OUTER_BOUND('',#2274,.T.);
#1613=FACE_OUTER_BOUND('',#2276,.T.);
#1614=FACE_OUTER_BOUND('',#2278,.T.);
#1615=FACE_OUTER_BOUND('',#2280,.T.);
#1616=FACE_OUTER_BOUND('',#2282,.T.);
#1617=FACE_OUTER_BOUND('',#2283,.T.);
#1618=FACE_OUTER_BOUND('',#2284,.T.);
#1619=FACE_OUTER_BOUND('',#2286,.T.);
#1620=FACE_OUTER_BOUND('',#2288,.T.);
#1621=FACE_OUTER_BOUND('',#2289,.T.);
#1622=FACE_OUTER_BOUND('',#2291,.T.);
#1623=FACE_OUTER_BOUND('',#2292,.T.);
#1624=FACE_OUTER_BOUND('',#2293,.T.);
#1625=FACE_OUTER_BOUND('',#2294,.T.);
#1626=FACE_OUTER_BOUND('',#2295,.T.);
#1627=FACE_OUTER_BOUND('',#2296,.T.);
#1628=FACE_OUTER_BOUND('',#2297,.T.);
#1629=FACE_OUTER_BOUND('',#2298,.T.);
#1630=FACE_OUTER_BOUND('',#2299,.T.);
#1631=FACE_OUTER_BOUND('',#2300,.T.);
#1632=FACE_OUTER_BOUND('',#2303,.T.);
#1633=FACE_OUTER_BOUND('',#2305,.T.);
#1634=FACE_OUTER_BOUND('',#2306,.T.);
#1635=FACE_OUTER_BOUND('',#2307,.T.);
#1636=FACE_OUTER_BOUND('',#2308,.T.);
#1637=FACE_OUTER_BOUND('',#2309,.T.);
#1638=FACE_OUTER_BOUND('',#2310,.T.);
#1639=FACE_OUTER_BOUND('',#2311,.T.);
#1640=FACE_OUTER_BOUND('',#2313,.T.);
#1641=FACE_OUTER_BOUND('',#2314,.T.);
#1642=FACE_OUTER_BOUND('',#2316,.T.);
#1643=FACE_OUTER_BOUND('',#2317,.T.);
#1644=FACE_OUTER_BOUND('',#2318,.T.);
#1645=FACE_OUTER_BOUND('',#2319,.T.);
#1646=FACE_OUTER_BOUND('',#2320,.T.);
#1647=FACE_OUTER_BOUND('',#2322,.T.);
#1648=FACE_OUTER_BOUND('',#2324,.T.);
#1649=FACE_OUTER_BOUND('',#2325,.T.);
#1650=FACE_OUTER_BOUND('',#2326,.T.);
#1651=FACE_OUTER_BOUND('',#2328,.T.);
#1652=FACE_OUTER_BOUND('',#2330,.T.);
#1653=FACE_OUTER_BOUND('',#2331,.T.);
#1654=FACE_OUTER_BOUND('',#2332,.T.);
#1655=FACE_OUTER_BOUND('',#2334,.T.);
#1656=FACE_OUTER_BOUND('',#2336,.T.);
#1657=FACE_OUTER_BOUND('',#2337,.T.);
#1658=FACE_OUTER_BOUND('',#2338,.T.);
#1659=FACE_OUTER_BOUND('',#2339,.T.);
#1660=FACE_OUTER_BOUND('',#2340,.T.);
#1661=FACE_OUTER_BOUND('',#2341,.T.);
#1662=FACE_OUTER_BOUND('',#2342,.T.);
#1663=FACE_OUTER_BOUND('',#2343,.T.);
#1664=FACE_OUTER_BOUND('',#2344,.T.);
#1665=FACE_OUTER_BOUND('',#2345,.T.);
#1666=FACE_OUTER_BOUND('',#2346,.T.);
#1667=FACE_OUTER_BOUND('',#2347,.T.);
#1668=FACE_OUTER_BOUND('',#2348,.T.);
#1669=FACE_OUTER_BOUND('',#2349,.T.);
#1670=FACE_OUTER_BOUND('',#2350,.T.);
#1671=FACE_OUTER_BOUND('',#2351,.T.);
#1672=FACE_OUTER_BOUND('',#2352,.T.);
#1673=FACE_OUTER_BOUND('',#2353,.T.);
#1674=FACE_OUTER_BOUND('',#2355,.T.);
#1675=FACE_OUTER_BOUND('',#2356,.T.);
#1676=FACE_OUTER_BOUND('',#2357,.T.);
#1677=FACE_OUTER_BOUND('',#2358,.T.);
#1678=FACE_OUTER_BOUND('',#2359,.T.);
#1679=FACE_OUTER_BOUND('',#2360,.T.);
#1680=FACE_OUTER_BOUND('',#2361,.T.);
#1681=FACE_OUTER_BOUND('',#2362,.T.);
#1682=FACE_OUTER_BOUND('',#2365,.T.);
#1683=FACE_OUTER_BOUND('',#2366,.T.);
#1684=FACE_OUTER_BOUND('',#2367,.T.);
#1685=FACE_OUTER_BOUND('',#2368,.T.);
#1686=FACE_OUTER_BOUND('',#2371,.T.);
#1687=FACE_OUTER_BOUND('',#2372,.T.);
#1688=FACE_OUTER_BOUND('',#2373,.T.);
#1689=FACE_OUTER_BOUND('',#2375,.T.);
#1690=FACE_OUTER_BOUND('',#2377,.T.);
#1691=FACE_OUTER_BOUND('',#2378,.T.);
#1692=FACE_OUTER_BOUND('',#2379,.T.);
#1693=FACE_OUTER_BOUND('',#2381,.T.);
#1694=FACE_OUTER_BOUND('',#2383,.T.);
#1695=FACE_OUTER_BOUND('',#2384,.T.);
#1696=FACE_OUTER_BOUND('',#2385,.T.);
#1697=FACE_OUTER_BOUND('',#2387,.T.);
#1698=FACE_OUTER_BOUND('',#2389,.T.);
#1699=FACE_OUTER_BOUND('',#2390,.T.);
#1700=FACE_OUTER_BOUND('',#2391,.T.);
#1701=FACE_OUTER_BOUND('',#2393,.T.);
#1702=FACE_OUTER_BOUND('',#2395,.T.);
#1703=FACE_OUTER_BOUND('',#2396,.T.);
#1704=FACE_OUTER_BOUND('',#2397,.T.);
#1705=FACE_OUTER_BOUND('',#2398,.T.);
#1706=FACE_OUTER_BOUND('',#2399,.T.);
#1707=FACE_OUTER_BOUND('',#2401,.T.);
#1708=FACE_OUTER_BOUND('',#2402,.T.);
#1709=FACE_OUTER_BOUND('',#2404,.T.);
#1710=FACE_OUTER_BOUND('',#2405,.T.);
#1711=FACE_OUTER_BOUND('',#2406,.T.);
#1712=FACE_OUTER_BOUND('',#2407,.T.);
#1713=FACE_OUTER_BOUND('',#2409,.T.);
#1714=FACE_OUTER_BOUND('',#2410,.T.);
#1715=FACE_OUTER_BOUND('',#2411,.T.);
#1716=FACE_OUTER_BOUND('',#2412,.T.);
#1717=FACE_OUTER_BOUND('',#2414,.T.);
#1718=FACE_OUTER_BOUND('',#2415,.T.);
#1719=FACE_OUTER_BOUND('',#2416,.T.);
#1720=FACE_OUTER_BOUND('',#2417,.T.);
#1721=FACE_OUTER_BOUND('',#2418,.T.);
#1722=FACE_OUTER_BOUND('',#2419,.T.);
#1723=FACE_OUTER_BOUND('',#2420,.T.);
#1724=FACE_OUTER_BOUND('',#2421,.T.);
#1725=FACE_OUTER_BOUND('',#2422,.T.);
#1726=FACE_OUTER_BOUND('',#2423,.T.);
#1727=FACE_OUTER_BOUND('',#2424,.T.);
#1728=FACE_OUTER_BOUND('',#2425,.T.);
#1729=FACE_OUTER_BOUND('',#2426,.T.);
#1730=FACE_OUTER_BOUND('',#2427,.T.);
#1731=FACE_OUTER_BOUND('',#2428,.T.);
#1732=FACE_OUTER_BOUND('',#2429,.T.);
#1733=FACE_OUTER_BOUND('',#2430,.T.);
#1734=FACE_OUTER_BOUND('',#2431,.T.);
#1735=FACE_OUTER_BOUND('',#2432,.T.);
#1736=FACE_OUTER_BOUND('',#2433,.T.);
#1737=FACE_OUTER_BOUND('',#2434,.T.);
#1738=FACE_OUTER_BOUND('',#2435,.T.);
#1739=FACE_OUTER_BOUND('',#2436,.T.);
#1740=FACE_OUTER_BOUND('',#2437,.T.);
#1741=FACE_OUTER_BOUND('',#2438,.T.);
#1742=FACE_OUTER_BOUND('',#2439,.T.);
#1743=FACE_OUTER_BOUND('',#2440,.T.);
#1744=FACE_OUTER_BOUND('',#2442,.T.);
#1745=FACE_OUTER_BOUND('',#2443,.T.);
#1746=FACE_OUTER_BOUND('',#2445,.T.);
#1747=FACE_OUTER_BOUND('',#2446,.T.);
#1748=FACE_OUTER_BOUND('',#2448,.T.);
#1749=FACE_OUTER_BOUND('',#2449,.T.);
#1750=FACE_OUTER_BOUND('',#2451,.T.);
#1751=FACE_OUTER_BOUND('',#2452,.T.);
#1752=FACE_OUTER_BOUND('',#2454,.T.);
#1753=FACE_OUTER_BOUND('',#2455,.T.);
#1754=FACE_OUTER_BOUND('',#2456,.T.);
#1755=FACE_OUTER_BOUND('',#2458,.T.);
#1756=FACE_OUTER_BOUND('',#2459,.T.);
#1757=FACE_OUTER_BOUND('',#2460,.T.);
#1758=FACE_OUTER_BOUND('',#2461,.T.);
#1759=FACE_OUTER_BOUND('',#2463,.T.);
#1760=FACE_OUTER_BOUND('',#2464,.T.);
#1761=FACE_OUTER_BOUND('',#2465,.T.);
#1762=FACE_OUTER_BOUND('',#2466,.T.);
#1763=FACE_OUTER_BOUND('',#2467,.T.);
#1764=FACE_OUTER_BOUND('',#2468,.T.);
#1765=FACE_OUTER_BOUND('',#2469,.T.);
#1766=FACE_OUTER_BOUND('',#2470,.T.);
#1767=FACE_OUTER_BOUND('',#2477,.T.);
#1768=FACE_OUTER_BOUND('',#2478,.T.);
#1769=FACE_OUTER_BOUND('',#2485,.T.);
#1770=FACE_OUTER_BOUND('',#2487,.T.);
#1771=FACE_OUTER_BOUND('',#2488,.T.);
#1772=FACE_OUTER_BOUND('',#2489,.T.);
#1773=FACE_OUTER_BOUND('',#2490,.T.);
#1774=FACE_OUTER_BOUND('',#2491,.T.);
#1775=FACE_OUTER_BOUND('',#2492,.T.);
#1776=FACE_OUTER_BOUND('',#2493,.T.);
#1777=FACE_OUTER_BOUND('',#2494,.T.);
#1778=FACE_OUTER_BOUND('',#2495,.T.);
#1779=FACE_OUTER_BOUND('',#2502,.T.);
#1780=FACE_OUTER_BOUND('',#2503,.T.);
#1781=FACE_OUTER_BOUND('',#2510,.T.);
#1782=FACE_OUTER_BOUND('',#2511,.T.);
#1783=FACE_OUTER_BOUND('',#2512,.T.);
#1784=FACE_OUTER_BOUND('',#2513,.T.);
#1785=FACE_OUTER_BOUND('',#2514,.T.);
#1786=FACE_OUTER_BOUND('',#2515,.T.);
#1787=FACE_OUTER_BOUND('',#2516,.T.);
#1788=FACE_OUTER_BOUND('',#2517,.T.);
#1789=FACE_OUTER_BOUND('',#2518,.T.);
#1790=FACE_OUTER_BOUND('',#2519,.T.);
#1791=FACE_OUTER_BOUND('',#2526,.T.);
#1792=FACE_OUTER_BOUND('',#2527,.T.);
#1793=FACE_OUTER_BOUND('',#2534,.T.);
#1794=FACE_OUTER_BOUND('',#2535,.T.);
#1795=FACE_OUTER_BOUND('',#2536,.T.);
#1796=FACE_OUTER_BOUND('',#2537,.T.);
#1797=FACE_OUTER_BOUND('',#2538,.T.);
#1798=FACE_OUTER_BOUND('',#2540,.T.);
#1799=FACE_OUTER_BOUND('',#2541,.T.);
#1800=FACE_OUTER_BOUND('',#2542,.T.);
#1801=FACE_OUTER_BOUND('',#2543,.T.);
#1802=FACE_OUTER_BOUND('',#2545,.T.);
#1803=FACE_OUTER_BOUND('',#2546,.T.);
#1804=FACE_OUTER_BOUND('',#2547,.T.);
#1805=FACE_OUTER_BOUND('',#2549,.T.);
#1806=FACE_OUTER_BOUND('',#2551,.T.);
#1807=FACE_OUTER_BOUND('',#2552,.T.);
#1808=FACE_OUTER_BOUND('',#2553,.T.);
#1809=FACE_OUTER_BOUND('',#2555,.T.);
#1810=FACE_OUTER_BOUND('',#2557,.T.);
#1811=FACE_OUTER_BOUND('',#2558,.T.);
#1812=FACE_OUTER_BOUND('',#2559,.T.);
#1813=FACE_OUTER_BOUND('',#2561,.T.);
#1814=FACE_OUTER_BOUND('',#2563,.T.);
#1815=FACE_OUTER_BOUND('',#2564,.T.);
#1816=FACE_OUTER_BOUND('',#2565,.T.);
#1817=FACE_OUTER_BOUND('',#2566,.T.);
#1818=FACE_OUTER_BOUND('',#2567,.T.);
#1819=FACE_OUTER_BOUND('',#2568,.T.);
#1820=FACE_OUTER_BOUND('',#2570,.T.);
#1821=FACE_OUTER_BOUND('',#2571,.T.);
#1822=FACE_OUTER_BOUND('',#2573,.T.);
#1823=FACE_OUTER_BOUND('',#2574,.T.);
#1824=FACE_OUTER_BOUND('',#2576,.T.);
#1825=FACE_OUTER_BOUND('',#2577,.T.);
#1826=FACE_OUTER_BOUND('',#2579,.T.);
#1827=FACE_OUTER_BOUND('',#2580,.T.);
#1828=FACE_OUTER_BOUND('',#2582,.T.);
#1829=FACE_OUTER_BOUND('',#2583,.T.);
#1830=FACE_OUTER_BOUND('',#2585,.T.);
#1831=FACE_OUTER_BOUND('',#2587,.T.);
#1832=FACE_OUTER_BOUND('',#2588,.T.);
#1833=FACE_OUTER_BOUND('',#2589,.T.);
#1834=FACE_OUTER_BOUND('',#2590,.T.);
#1835=FACE_OUTER_BOUND('',#2591,.T.);
#1836=FACE_OUTER_BOUND('',#2593,.T.);
#1837=FACE_OUTER_BOUND('',#2595,.T.);
#1838=FACE_OUTER_BOUND('',#2597,.T.);
#1839=FACE_OUTER_BOUND('',#2599,.T.);
#1840=FACE_OUTER_BOUND('',#2600,.T.);
#1841=FACE_OUTER_BOUND('',#2601,.T.);
#1842=FACE_OUTER_BOUND('',#2602,.T.);
#1843=FACE_OUTER_BOUND('',#2603,.T.);
#1844=FACE_OUTER_BOUND('',#2604,.T.);
#1845=FACE_OUTER_BOUND('',#2605,.T.);
#1846=FACE_OUTER_BOUND('',#2606,.T.);
#1847=FACE_OUTER_BOUND('',#2607,.T.);
#1848=FACE_OUTER_BOUND('',#2608,.T.);
#1849=FACE_OUTER_BOUND('',#2609,.T.);
#1850=FACE_OUTER_BOUND('',#2610,.T.);
#1851=FACE_OUTER_BOUND('',#2611,.T.);
#1852=FACE_OUTER_BOUND('',#2612,.T.);
#1853=FACE_OUTER_BOUND('',#2614,.T.);
#1854=FACE_OUTER_BOUND('',#2615,.T.);
#1855=EDGE_LOOP('',(#6122,#6123,#6124,#6125));
#1856=EDGE_LOOP('',(#6126,#6127,#6128,#6129));
#1857=EDGE_LOOP('',(#6130,#6131,#6132,#6133));
#1858=EDGE_LOOP('',(#6134,#6135,#6136,#6137));
#1859=EDGE_LOOP('',(#6138,#6139,#6140,#6141));
#1860=EDGE_LOOP('',(#6142,#6143,#6144,#6145));
#1861=EDGE_LOOP('',(#6146,#6147,#6148,#6149));
#1862=EDGE_LOOP('',(#6150,#6151,#6152,#6153));
#1863=EDGE_LOOP('',(#6154,#6155,#6156,#6157));
#1864=EDGE_LOOP('',(#6158,#6159,#6160,#6161));
#1865=EDGE_LOOP('',(#6162,#6163,#6164,#6165));
#1866=EDGE_LOOP('',(#6166,#6167,#6168,#6169));
#1867=EDGE_LOOP('',(#6170,#6171,#6172,#6173));
#1868=EDGE_LOOP('',(#6174,#6175,#6176,#6177));
#1869=EDGE_LOOP('',(#6178,#6179,#6180,#6181));
#1870=EDGE_LOOP('',(#6182,#6183,#6184,#6185));
#1871=EDGE_LOOP('',(#6186,#6187,#6188,#6189));
#1872=EDGE_LOOP('',(#6190));
#1873=EDGE_LOOP('',(#6191));
#1874=EDGE_LOOP('',(#6192));
#1875=EDGE_LOOP('',(#6193));
#1876=EDGE_LOOP('',(#6194));
#1877=EDGE_LOOP('',(#6195));
#1878=EDGE_LOOP('',(#6196));
#1879=EDGE_LOOP('',(#6197));
#1880=EDGE_LOOP('',(#6198));
#1881=EDGE_LOOP('',(#6199));
#1882=EDGE_LOOP('',(#6200));
#1883=EDGE_LOOP('',(#6201));
#1884=EDGE_LOOP('',(#6202,#6203,#6204,#6205));
#1885=EDGE_LOOP('',(#6206));
#1886=EDGE_LOOP('',(#6207));
#1887=EDGE_LOOP('',(#6208));
#1888=EDGE_LOOP('',(#6209));
#1889=EDGE_LOOP('',(#6210));
#1890=EDGE_LOOP('',(#6211));
#1891=EDGE_LOOP('',(#6212));
#1892=EDGE_LOOP('',(#6213));
#1893=EDGE_LOOP('',(#6214));
#1894=EDGE_LOOP('',(#6215));
#1895=EDGE_LOOP('',(#6216));
#1896=EDGE_LOOP('',(#6217));
#1897=EDGE_LOOP('',(#6218,#6219,#6220,#6221));
#1898=EDGE_LOOP('',(#6222));
#1899=EDGE_LOOP('',(#6223,#6224,#6225,#6226));
#1900=EDGE_LOOP('',(#6227));
#1901=EDGE_LOOP('',(#6228,#6229,#6230,#6231));
#1902=EDGE_LOOP('',(#6232));
#1903=EDGE_LOOP('',(#6233));
#1904=EDGE_LOOP('',(#6234,#6235,#6236,#6237));
#1905=EDGE_LOOP('',(#6238));
#1906=EDGE_LOOP('',(#6239));
#1907=EDGE_LOOP('',(#6240,#6241,#6242,#6243));
#1908=EDGE_LOOP('',(#6244));
#1909=EDGE_LOOP('',(#6245));
#1910=EDGE_LOOP('',(#6246,#6247,#6248,#6249));
#1911=EDGE_LOOP('',(#6250));
#1912=EDGE_LOOP('',(#6251));
#1913=EDGE_LOOP('',(#6252,#6253,#6254,#6255));
#1914=EDGE_LOOP('',(#6256,#6257,#6258,#6259));
#1915=EDGE_LOOP('',(#6260,#6261,#6262,#6263));
#1916=EDGE_LOOP('',(#6264,#6265,#6266,#6267));
#1917=EDGE_LOOP('',(#6268,#6269,#6270,#6271));
#1918=EDGE_LOOP('',(#6272,#6273,#6274,#6275));
#1919=EDGE_LOOP('',(#6276,#6277,#6278,#6279));
#1920=EDGE_LOOP('',(#6280,#6281,#6282,#6283));
#1921=EDGE_LOOP('',(#6284,#6285,#6286,#6287));
#1922=EDGE_LOOP('',(#6288));
#1923=EDGE_LOOP('',(#6289));
#1924=EDGE_LOOP('',(#6290));
#1925=EDGE_LOOP('',(#6291));
#1926=EDGE_LOOP('',(#6292));
#1927=EDGE_LOOP('',(#6293));
#1928=EDGE_LOOP('',(#6294,#6295,#6296,#6297));
#1929=EDGE_LOOP('',(#6298));
#1930=EDGE_LOOP('',(#6299));
#1931=EDGE_LOOP('',(#6300));
#1932=EDGE_LOOP('',(#6301));
#1933=EDGE_LOOP('',(#6302,#6303,#6304,#6305));
#1934=EDGE_LOOP('',(#6306,#6307,#6308,#6309));
#1935=EDGE_LOOP('',(#6310));
#1936=EDGE_LOOP('',(#6311));
#1937=EDGE_LOOP('',(#6312));
#1938=EDGE_LOOP('',(#6313));
#1939=EDGE_LOOP('',(#6314,#6315,#6316,#6317));
#1940=EDGE_LOOP('',(#6318,#6319,#6320,#6321));
#1941=EDGE_LOOP('',(#6322));
#1942=EDGE_LOOP('',(#6323));
#1943=EDGE_LOOP('',(#6324));
#1944=EDGE_LOOP('',(#6325));
#1945=EDGE_LOOP('',(#6326,#6327,#6328,#6329));
#1946=EDGE_LOOP('',(#6330));
#1947=EDGE_LOOP('',(#6331,#6332,#6333,#6334));
#1948=EDGE_LOOP('',(#6335));
#1949=EDGE_LOOP('',(#6336,#6337,#6338,#6339));
#1950=EDGE_LOOP('',(#6340));
#1951=EDGE_LOOP('',(#6341));
#1952=EDGE_LOOP('',(#6342,#6343,#6344,#6345));
#1953=EDGE_LOOP('',(#6346));
#1954=EDGE_LOOP('',(#6347));
#1955=EDGE_LOOP('',(#6348,#6349,#6350,#6351));
#1956=EDGE_LOOP('',(#6352));
#1957=EDGE_LOOP('',(#6353));
#1958=EDGE_LOOP('',(#6354,#6355,#6356,#6357));
#1959=EDGE_LOOP('',(#6358));
#1960=EDGE_LOOP('',(#6359));
#1961=EDGE_LOOP('',(#6360,#6361,#6362,#6363));
#1962=EDGE_LOOP('',(#6364,#6365,#6366,#6367));
#1963=EDGE_LOOP('',(#6368,#6369,#6370,#6371));
#1964=EDGE_LOOP('',(#6372,#6373,#6374,#6375));
#1965=EDGE_LOOP('',(#6376,#6377,#6378,#6379));
#1966=EDGE_LOOP('',(#6380,#6381,#6382,#6383));
#1967=EDGE_LOOP('',(#6384,#6385,#6386,#6387));
#1968=EDGE_LOOP('',(#6388,#6389,#6390,#6391));
#1969=EDGE_LOOP('',(#6392,#6393,#6394,#6395));
#1970=EDGE_LOOP('',(#6396));
#1971=EDGE_LOOP('',(#6397));
#1972=EDGE_LOOP('',(#6398));
#1973=EDGE_LOOP('',(#6399));
#1974=EDGE_LOOP('',(#6400));
#1975=EDGE_LOOP('',(#6401));
#1976=EDGE_LOOP('',(#6402,#6403,#6404,#6405));
#1977=EDGE_LOOP('',(#6406));
#1978=EDGE_LOOP('',(#6407));
#1979=EDGE_LOOP('',(#6408));
#1980=EDGE_LOOP('',(#6409));
#1981=EDGE_LOOP('',(#6410,#6411,#6412,#6413));
#1982=EDGE_LOOP('',(#6414,#6415,#6416,#6417));
#1983=EDGE_LOOP('',(#6418));
#1984=EDGE_LOOP('',(#6419));
#1985=EDGE_LOOP('',(#6420));
#1986=EDGE_LOOP('',(#6421));
#1987=EDGE_LOOP('',(#6422,#6423,#6424,#6425));
#1988=EDGE_LOOP('',(#6426,#6427,#6428,#6429));
#1989=EDGE_LOOP('',(#6430));
#1990=EDGE_LOOP('',(#6431));
#1991=EDGE_LOOP('',(#6432));
#1992=EDGE_LOOP('',(#6433));
#1993=EDGE_LOOP('',(#6434,#6435,#6436,#6437));
#1994=EDGE_LOOP('',(#6438,#6439,#6440,#6441));
#1995=EDGE_LOOP('',(#6442));
#1996=EDGE_LOOP('',(#6443));
#1997=EDGE_LOOP('',(#6444,#6445,#6446,#6447));
#1998=EDGE_LOOP('',(#6448,#6449));
#1999=EDGE_LOOP('',(#6450));
#2000=EDGE_LOOP('',(#6451,#6452,#6453,#6454,#6455,#6456,#6457,#6458,#6459));
#2001=EDGE_LOOP('',(#6460));
#2002=EDGE_LOOP('',(#6461));
#2003=EDGE_LOOP('',(#6462));
#2004=EDGE_LOOP('',(#6463));
#2005=EDGE_LOOP('',(#6464,#6465,#6466,#6467));
#2006=EDGE_LOOP('',(#6468,#6469,#6470,#6471));
#2007=EDGE_LOOP('',(#6472,#6473,#6474,#6475));
#2008=EDGE_LOOP('',(#6476));
#2009=EDGE_LOOP('',(#6477,#6478,#6479,#6480));
#2010=EDGE_LOOP('',(#6481));
#2011=EDGE_LOOP('',(#6482,#6483,#6484,#6485));
#2012=EDGE_LOOP('',(#6486));
#2013=EDGE_LOOP('',(#6487,#6488,#6489,#6490));
#2014=EDGE_LOOP('',(#6491));
#2015=EDGE_LOOP('',(#6492,#6493,#6494,#6495));
#2016=EDGE_LOOP('',(#6496,#6497,#6498,#6499,#6500,#6501,#6502));
#2017=EDGE_LOOP('',(#6503,#6504,#6505,#6506));
#2018=EDGE_LOOP('',(#6507,#6508,#6509,#6510,#6511,#6512,#6513));
#2019=EDGE_LOOP('',(#6514,#6515,#6516,#6517));
#2020=EDGE_LOOP('',(#6518));
#2021=EDGE_LOOP('',(#6519));
#2022=EDGE_LOOP('',(#6520,#6521,#6522,#6523));
#2023=EDGE_LOOP('',(#6524,#6525,#6526,#6527));
#2024=EDGE_LOOP('',(#6528));
#2025=EDGE_LOOP('',(#6529));
#2026=EDGE_LOOP('',(#6530,#6531,#6532,#6533));
#2027=EDGE_LOOP('',(#6534,#6535));
#2028=EDGE_LOOP('',(#6536));
#2029=EDGE_LOOP('',(#6537,#6538,#6539,#6540,#6541,#6542,#6543,#6544,#6545));
#2030=EDGE_LOOP('',(#6546));
#2031=EDGE_LOOP('',(#6547));
#2032=EDGE_LOOP('',(#6548));
#2033=EDGE_LOOP('',(#6549));
#2034=EDGE_LOOP('',(#6550,#6551,#6552,#6553));
#2035=EDGE_LOOP('',(#6554,#6555,#6556,#6557));
#2036=EDGE_LOOP('',(#6558,#6559,#6560,#6561));
#2037=EDGE_LOOP('',(#6562));
#2038=EDGE_LOOP('',(#6563,#6564,#6565,#6566));
#2039=EDGE_LOOP('',(#6567));
#2040=EDGE_LOOP('',(#6568,#6569,#6570,#6571));
#2041=EDGE_LOOP('',(#6572));
#2042=EDGE_LOOP('',(#6573,#6574,#6575,#6576));
#2043=EDGE_LOOP('',(#6577));
#2044=EDGE_LOOP('',(#6578,#6579,#6580,#6581));
#2045=EDGE_LOOP('',(#6582,#6583,#6584,#6585,#6586,#6587,#6588));
#2046=EDGE_LOOP('',(#6589,#6590,#6591,#6592));
#2047=EDGE_LOOP('',(#6593,#6594,#6595,#6596,#6597,#6598,#6599));
#2048=EDGE_LOOP('',(#6600,#6601,#6602,#6603));
#2049=EDGE_LOOP('',(#6604));
#2050=EDGE_LOOP('',(#6605));
#2051=EDGE_LOOP('',(#6606,#6607,#6608,#6609));
#2052=EDGE_LOOP('',(#6610,#6611,#6612,#6613));
#2053=EDGE_LOOP('',(#6614,#6615,#6616,#6617));
#2054=EDGE_LOOP('',(#6618,#6619,#6620,#6621));
#2055=EDGE_LOOP('',(#6622,#6623,#6624,#6625));
#2056=EDGE_LOOP('',(#6626,#6627,#6628,#6629));
#2057=EDGE_LOOP('',(#6630,#6631,#6632,#6633));
#2058=EDGE_LOOP('',(#6634,#6635,#6636,#6637));
#2059=EDGE_LOOP('',(#6638,#6639,#6640,#6641));
#2060=EDGE_LOOP('',(#6642,#6643,#6644,#6645));
#2061=EDGE_LOOP('',(#6646,#6647,#6648,#6649));
#2062=EDGE_LOOP('',(#6650,#6651,#6652,#6653));
#2063=EDGE_LOOP('',(#6654));
#2064=EDGE_LOOP('',(#6655,#6656,#6657,#6658));
#2065=EDGE_LOOP('',(#6659,#6660,#6661,#6662));
#2066=EDGE_LOOP('',(#6663,#6664,#6665,#6666));
#2067=EDGE_LOOP('',(#6667));
#2068=EDGE_LOOP('',(#6668));
#2069=EDGE_LOOP('',(#6669,#6670,#6671,#6672));
#2070=EDGE_LOOP('',(#6673,#6674,#6675,#6676));
#2071=EDGE_LOOP('',(#6677,#6678,#6679,#6680));
#2072=EDGE_LOOP('',(#6681));
#2073=EDGE_LOOP('',(#6682,#6683,#6684,#6685));
#2074=EDGE_LOOP('',(#6686,#6687,#6688,#6689));
#2075=EDGE_LOOP('',(#6690,#6691,#6692,#6693));
#2076=EDGE_LOOP('',(#6694,#6695,#6696,#6697));
#2077=EDGE_LOOP('',(#6698,#6699,#6700,#6701));
#2078=EDGE_LOOP('',(#6702,#6703,#6704,#6705));
#2079=EDGE_LOOP('',(#6706,#6707,#6708,#6709,#6710,#6711));
#2080=EDGE_LOOP('',(#6712,#6713,#6714,#6715,#6716,#6717));
#2081=EDGE_LOOP('',(#6718,#6719,#6720,#6721));
#2082=EDGE_LOOP('',(#6722,#6723,#6724,#6725));
#2083=EDGE_LOOP('',(#6726,#6727));
#2084=EDGE_LOOP('',(#6728));
#2085=EDGE_LOOP('',(#6729));
#2086=EDGE_LOOP('',(#6730,#6731,#6732));
#2087=EDGE_LOOP('',(#6733,#6734,#6735));
#2088=EDGE_LOOP('',(#6736,#6737,#6738));
#2089=EDGE_LOOP('',(#6739,#6740,#6741,#6742));
#2090=EDGE_LOOP('',(#6743,#6744,#6745));
#2091=EDGE_LOOP('',(#6746,#6747,#6748,#6749));
#2092=EDGE_LOOP('',(#6750,#6751,#6752,#6753));
#2093=EDGE_LOOP('',(#6754));
#2094=EDGE_LOOP('',(#6755));
#2095=EDGE_LOOP('',(#6756,#6757,#6758,#6759,#6760,#6761,#6762,#6763,#6764,
#6765,#6766,#6767));
#2096=EDGE_LOOP('',(#6768,#6769,#6770,#6771,#6772,#6773,#6774,#6775,#6776,
#6777,#6778,#6779));
#2097=EDGE_LOOP('',(#6780,#6781));
#2098=EDGE_LOOP('',(#6782));
#2099=EDGE_LOOP('',(#6783,#6784));
#2100=EDGE_LOOP('',(#6785));
#2101=EDGE_LOOP('',(#6786,#6787,#6788,#6789));
#2102=EDGE_LOOP('',(#6790,#6791,#6792,#6793));
#2103=EDGE_LOOP('',(#6794,#6795,#6796,#6797));
#2104=EDGE_LOOP('',(#6798,#6799,#6800,#6801));
#2105=EDGE_LOOP('',(#6802,#6803,#6804,#6805));
#2106=EDGE_LOOP('',(#6806,#6807,#6808,#6809));
#2107=EDGE_LOOP('',(#6810,#6811,#6812,#6813));
#2108=EDGE_LOOP('',(#6814,#6815,#6816,#6817));
#2109=EDGE_LOOP('',(#6818,#6819,#6820,#6821));
#2110=EDGE_LOOP('',(#6822,#6823,#6824,#6825));
#2111=EDGE_LOOP('',(#6826,#6827,#6828,#6829));
#2112=EDGE_LOOP('',(#6830,#6831,#6832,#6833));
#2113=EDGE_LOOP('',(#6834,#6835,#6836,#6837));
#2114=EDGE_LOOP('',(#6838));
#2115=EDGE_LOOP('',(#6839));
#2116=EDGE_LOOP('',(#6840,#6841,#6842,#6843));
#2117=EDGE_LOOP('',(#6844));
#2118=EDGE_LOOP('',(#6845));
#2119=EDGE_LOOP('',(#6846,#6847));
#2120=EDGE_LOOP('',(#6848));
#2121=EDGE_LOOP('',(#6849));
#2122=EDGE_LOOP('',(#6850));
#2123=EDGE_LOOP('',(#6851));
#2124=EDGE_LOOP('',(#6852,#6853,#6854,#6855,#6856,#6857));
#2125=EDGE_LOOP('',(#6858,#6859,#6860,#6861,#6862,#6863));
#2126=EDGE_LOOP('',(#6864,#6865,#6866,#6867));
#2127=EDGE_LOOP('',(#6868,#6869,#6870));
#2128=EDGE_LOOP('',(#6871,#6872,#6873));
#2129=EDGE_LOOP('',(#6874,#6875,#6876));
#2130=EDGE_LOOP('',(#6877,#6878,#6879));
#2131=EDGE_LOOP('',(#6880,#6881,#6882));
#2132=EDGE_LOOP('',(#6883,#6884,#6885));
#2133=EDGE_LOOP('',(#6886,#6887,#6888,#6889,#6890,#6891));
#2134=EDGE_LOOP('',(#6892,#6893,#6894,#6895,#6896,#6897));
#2135=EDGE_LOOP('',(#6898,#6899,#6900,#6901,#6902,#6903));
#2136=EDGE_LOOP('',(#6904,#6905,#6906,#6907,#6908,#6909));
#2137=EDGE_LOOP('',(#6910));
#2138=EDGE_LOOP('',(#6911));
#2139=EDGE_LOOP('',(#6912));
#2140=EDGE_LOOP('',(#6913));
#2141=EDGE_LOOP('',(#6914,#6915,#6916,#6917));
#2142=EDGE_LOOP('',(#6918));
#2143=EDGE_LOOP('',(#6919));
#2144=EDGE_LOOP('',(#6920,#6921,#6922,#6923));
#2145=EDGE_LOOP('',(#6924));
#2146=EDGE_LOOP('',(#6925));
#2147=EDGE_LOOP('',(#6926));
#2148=EDGE_LOOP('',(#6927));
#2149=EDGE_LOOP('',(#6928));
#2150=EDGE_LOOP('',(#6929));
#2151=EDGE_LOOP('',(#6930,#6931,#6932,#6933));
#2152=EDGE_LOOP('',(#6934,#6935,#6936,#6937));
#2153=EDGE_LOOP('',(#6938));
#2154=EDGE_LOOP('',(#6939));
#2155=EDGE_LOOP('',(#6940));
#2156=EDGE_LOOP('',(#6941));
#2157=EDGE_LOOP('',(#6942,#6943,#6944,#6945));
#2158=EDGE_LOOP('',(#6946,#6947,#6948,#6949));
#2159=EDGE_LOOP('',(#6950,#6951,#6952,#6953));
#2160=EDGE_LOOP('',(#6954,#6955,#6956,#6957));
#2161=EDGE_LOOP('',(#6958,#6959,#6960,#6961));
#2162=EDGE_LOOP('',(#6962,#6963,#6964,#6965));
#2163=EDGE_LOOP('',(#6966,#6967,#6968,#6969,#6970,#6971));
#2164=EDGE_LOOP('',(#6972,#6973,#6974,#6975,#6976,#6977));
#2165=EDGE_LOOP('',(#6978));
#2166=EDGE_LOOP('',(#6979));
#2167=EDGE_LOOP('',(#6980,#6981,#6982,#6983));
#2168=EDGE_LOOP('',(#6984,#6985,#6986,#6987));
#2169=EDGE_LOOP('',(#6988,#6989,#6990,#6991));
#2170=EDGE_LOOP('',(#6992));
#2171=EDGE_LOOP('',(#6993));
#2172=EDGE_LOOP('',(#6994,#6995,#6996,#6997));
#2173=EDGE_LOOP('',(#6998,#6999,#7000,#7001));
#2174=EDGE_LOOP('',(#7002,#7003));
#2175=EDGE_LOOP('',(#7004,#7005,#7006,#7007));
#2176=EDGE_LOOP('',(#7008,#7009,#7010,#7011));
#2177=EDGE_LOOP('',(#7012,#7013));
#2178=EDGE_LOOP('',(#7014,#7015,#7016,#7017,#7018,#7019));
#2179=EDGE_LOOP('',(#7020));
#2180=EDGE_LOOP('',(#7021,#7022,#7023,#7024,#7025,#7026,#7027,#7028));
#2181=EDGE_LOOP('',(#7029));
#2182=EDGE_LOOP('',(#7030,#7031,#7032,#7033,#7034,#7035));
#2183=EDGE_LOOP('',(#7036));
#2184=EDGE_LOOP('',(#7037,#7038,#7039,#7040));
#2185=EDGE_LOOP('',(#7041,#7042,#7043,#7044));
#2186=EDGE_LOOP('',(#7045,#7046,#7047,#7048));
#2187=EDGE_LOOP('',(#7049,#7050,#7051,#7052));
#2188=EDGE_LOOP('',(#7053,#7054,#7055,#7056));
#2189=EDGE_LOOP('',(#7057,#7058,#7059,#7060,#7061,#7062,#7063,#7064,#7065,
#7066,#7067,#7068));
#2190=EDGE_LOOP('',(#7069));
#2191=EDGE_LOOP('',(#7070,#7071,#7072,#7073));
#2192=EDGE_LOOP('',(#7074,#7075,#7076,#7077));
#2193=EDGE_LOOP('',(#7078));
#2194=EDGE_LOOP('',(#7079));
#2195=EDGE_LOOP('',(#7080,#7081,#7082,#7083));
#2196=EDGE_LOOP('',(#7084,#7085,#7086,#7087,#7088,#7089,#7090,#7091));
#2197=EDGE_LOOP('',(#7092));
#2198=EDGE_LOOP('',(#7093,#7094,#7095,#7096));
#2199=EDGE_LOOP('',(#7097,#7098,#7099,#7100));
#2200=EDGE_LOOP('',(#7101));
#2201=EDGE_LOOP('',(#7102,#7103,#7104,#7105));
#2202=EDGE_LOOP('',(#7106,#7107,#7108,#7109));
#2203=EDGE_LOOP('',(#7110));
#2204=EDGE_LOOP('',(#7111,#7112,#7113,#7114));
#2205=EDGE_LOOP('',(#7115,#7116,#7117,#7118,#7119,#7120,#7121,#7122,#7123,
#7124,#7125,#7126));
#2206=EDGE_LOOP('',(#7127));
#2207=EDGE_LOOP('',(#7128,#7129,#7130,#7131));
#2208=EDGE_LOOP('',(#7132,#7133,#7134,#7135));
#2209=EDGE_LOOP('',(#7136));
#2210=EDGE_LOOP('',(#7137));
#2211=EDGE_LOOP('',(#7138,#7139,#7140,#7141));
#2212=EDGE_LOOP('',(#7142));
#2213=EDGE_LOOP('',(#7143));
#2214=EDGE_LOOP('',(#7144,#7145,#7146,#7147));
#2215=EDGE_LOOP('',(#7148,#7149,#7150,#7151));
#2216=EDGE_LOOP('',(#7152,#7153,#7154,#7155));
#2217=EDGE_LOOP('',(#7156,#7157,#7158,#7159));
#2218=EDGE_LOOP('',(#7160,#7161,#7162,#7163));
#2219=EDGE_LOOP('',(#7164,#7165,#7166,#7167));
#2220=EDGE_LOOP('',(#7168,#7169,#7170,#7171,#7172,#7173));
#2221=EDGE_LOOP('',(#7174,#7175,#7176,#7177,#7178,#7179));
#2222=EDGE_LOOP('',(#7180));
#2223=EDGE_LOOP('',(#7181));
#2224=EDGE_LOOP('',(#7182,#7183,#7184,#7185));
#2225=EDGE_LOOP('',(#7186,#7187,#7188,#7189));
#2226=EDGE_LOOP('',(#7190,#7191,#7192,#7193));
#2227=EDGE_LOOP('',(#7194));
#2228=EDGE_LOOP('',(#7195));
#2229=EDGE_LOOP('',(#7196,#7197,#7198,#7199));
#2230=EDGE_LOOP('',(#7200,#7201,#7202,#7203));
#2231=EDGE_LOOP('',(#7204));
#2232=EDGE_LOOP('',(#7205,#7206,#7207,#7208));
#2233=EDGE_LOOP('',(#7209,#7210,#7211,#7212));
#2234=EDGE_LOOP('',(#7213,#7214,#7215,#7216));
#2235=EDGE_LOOP('',(#7217));
#2236=EDGE_LOOP('',(#7218));
#2237=EDGE_LOOP('',(#7219,#7220,#7221,#7222));
#2238=EDGE_LOOP('',(#7223,#7224,#7225,#7226));
#2239=EDGE_LOOP('',(#7227,#7228,#7229,#7230));
#2240=EDGE_LOOP('',(#7231));
#2241=EDGE_LOOP('',(#7232,#7233,#7234,#7235));
#2242=EDGE_LOOP('',(#7236,#7237,#7238,#7239));
#2243=EDGE_LOOP('',(#7240,#7241,#7242,#7243));
#2244=EDGE_LOOP('',(#7244,#7245,#7246,#7247));
#2245=EDGE_LOOP('',(#7248,#7249,#7250,#7251));
#2246=EDGE_LOOP('',(#7252,#7253,#7254,#7255));
#2247=EDGE_LOOP('',(#7256,#7257,#7258,#7259,#7260,#7261));
#2248=EDGE_LOOP('',(#7262,#7263,#7264,#7265,#7266,#7267));
#2249=EDGE_LOOP('',(#7268));
#2250=EDGE_LOOP('',(#7269,#7270,#7271,#7272));
#2251=EDGE_LOOP('',(#7273,#7274,#7275,#7276));
#2252=EDGE_LOOP('',(#7277));
#2253=EDGE_LOOP('',(#7278,#7279,#7280,#7281));
#2254=EDGE_LOOP('',(#7282,#7283,#7284,#7285));
#2255=EDGE_LOOP('',(#7286,#7287,#7288,#7289));
#2256=EDGE_LOOP('',(#7290,#7291,#7292,#7293));
#2257=EDGE_LOOP('',(#7294,#7295,#7296,#7297,#7298,#7299,#7300,#7301));
#2258=EDGE_LOOP('',(#7302,#7303,#7304,#7305,#7306));
#2259=EDGE_LOOP('',(#7307));
#2260=EDGE_LOOP('',(#7308,#7309));
#2261=EDGE_LOOP('',(#7310,#7311,#7312,#7313,#7314,#7315,#7316,#7317,#7318));
#2262=EDGE_LOOP('',(#7319,#7320,#7321));
#2263=EDGE_LOOP('',(#7322,#7323,#7324,#7325));
#2264=EDGE_LOOP('',(#7326,#7327,#7328,#7329));
#2265=EDGE_LOOP('',(#7330,#7331,#7332,#7333));
#2266=EDGE_LOOP('',(#7334,#7335));
#2267=EDGE_LOOP('',(#7336));
#2268=EDGE_LOOP('',(#7337));
#2269=EDGE_LOOP('',(#7338));
#2270=EDGE_LOOP('',(#7339));
#2271=EDGE_LOOP('',(#7340,#7341));
#2272=EDGE_LOOP('',(#7342,#7343,#7344,#7345,#7346,#7347,#7348,#7349,#7350));
#2273=EDGE_LOOP('',(#7351,#7352,#7353));
#2274=EDGE_LOOP('',(#7354,#7355,#7356,#7357));
#2275=EDGE_LOOP('',(#7358,#7359,#7360,#7361));
#2276=EDGE_LOOP('',(#7362,#7363,#7364,#7365));
#2277=EDGE_LOOP('',(#7366,#7367));
#2278=EDGE_LOOP('',(#7368));
#2279=EDGE_LOOP('',(#7369));
#2280=EDGE_LOOP('',(#7370));
#2281=EDGE_LOOP('',(#7371));
#2282=EDGE_LOOP('',(#7372,#7373,#7374,#7375));
#2283=EDGE_LOOP('',(#7376,#7377,#7378,#7379));
#2284=EDGE_LOOP('',(#7380));
#2285=EDGE_LOOP('',(#7381));
#2286=EDGE_LOOP('',(#7382));
#2287=EDGE_LOOP('',(#7383));
#2288=EDGE_LOOP('',(#7384,#7385,#7386,#7387));
#2289=EDGE_LOOP('',(#7388,#7389));
#2290=EDGE_LOOP('',(#7390,#7391,#7392,#7393));
#2291=EDGE_LOOP('',(#7394,#7395,#7396,#7397));
#2292=EDGE_LOOP('',(#7398));
#2293=EDGE_LOOP('',(#7399,#7400));
#2294=EDGE_LOOP('',(#7401,#7402,#7403,#7404,#7405,#7406,#7407,#7408));
#2295=EDGE_LOOP('',(#7409,#7410));
#2296=EDGE_LOOP('',(#7411,#7412,#7413,#7414,#7415,#7416,#7417,#7418,#7419,
#7420));
#2297=EDGE_LOOP('',(#7421,#7422,#7423,#7424));
#2298=EDGE_LOOP('',(#7425,#7426,#7427,#7428));
#2299=EDGE_LOOP('',(#7429,#7430,#7431,#7432));
#2300=EDGE_LOOP('',(#7433));
#2301=EDGE_LOOP('',(#7434));
#2302=EDGE_LOOP('',(#7435,#7436));
#2303=EDGE_LOOP('',(#7437));
#2304=EDGE_LOOP('',(#7438));
#2305=EDGE_LOOP('',(#7439,#7440,#7441,#7442));
#2306=EDGE_LOOP('',(#7443,#7444,#7445,#7446,#7447,#7448));
#2307=EDGE_LOOP('',(#7449,#7450,#7451,#7452));
#2308=EDGE_LOOP('',(#7453,#7454,#7455,#7456,#7457,#7458,#7459,#7460,#7461));
#2309=EDGE_LOOP('',(#7462,#7463,#7464,#7465));
#2310=EDGE_LOOP('',(#7466));
#2311=EDGE_LOOP('',(#7467));
#2312=EDGE_LOOP('',(#7468));
#2313=EDGE_LOOP('',(#7469,#7470,#7471,#7472));
#2314=EDGE_LOOP('',(#7473));
#2315=EDGE_LOOP('',(#7474));
#2316=EDGE_LOOP('',(#7475,#7476,#7477,#7478));
#2317=EDGE_LOOP('',(#7479));
#2318=EDGE_LOOP('',(#7480,#7481,#7482,#7483));
#2319=EDGE_LOOP('',(#7484,#7485,#7486,#7487));
#2320=EDGE_LOOP('',(#7488));
#2321=EDGE_LOOP('',(#7489));
#2322=EDGE_LOOP('',(#7490));
#2323=EDGE_LOOP('',(#7491));
#2324=EDGE_LOOP('',(#7492,#7493,#7494,#7495));
#2325=EDGE_LOOP('',(#7496,#7497,#7498,#7499));
#2326=EDGE_LOOP('',(#7500));
#2327=EDGE_LOOP('',(#7501));
#2328=EDGE_LOOP('',(#7502));
#2329=EDGE_LOOP('',(#7503));
#2330=EDGE_LOOP('',(#7504,#7505,#7506,#7507));
#2331=EDGE_LOOP('',(#7508,#7509,#7510,#7511));
#2332=EDGE_LOOP('',(#7512));
#2333=EDGE_LOOP('',(#7513));
#2334=EDGE_LOOP('',(#7514));
#2335=EDGE_LOOP('',(#7515));
#2336=EDGE_LOOP('',(#7516,#7517,#7518,#7519,#7520,#7521,#7522,#7523));
#2337=EDGE_LOOP('',(#7524,#7525,#7526,#7527));
#2338=EDGE_LOOP('',(#7528,#7529,#7530,#7531));
#2339=EDGE_LOOP('',(#7532,#7533,#7534,#7535));
#2340=EDGE_LOOP('',(#7536,#7537,#7538,#7539));
#2341=EDGE_LOOP('',(#7540,#7541,#7542,#7543,#7544,#7545,#7546,#7547));
#2342=EDGE_LOOP('',(#7548,#7549,#7550,#7551));
#2343=EDGE_LOOP('',(#7552,#7553,#7554,#7555));
#2344=EDGE_LOOP('',(#7556,#7557,#7558,#7559));
#2345=EDGE_LOOP('',(#7560,#7561,#7562,#7563));
#2346=EDGE_LOOP('',(#7564,#7565,#7566,#7567));
#2347=EDGE_LOOP('',(#7568,#7569,#7570,#7571));
#2348=EDGE_LOOP('',(#7572,#7573,#7574,#7575));
#2349=EDGE_LOOP('',(#7576,#7577,#7578,#7579));
#2350=EDGE_LOOP('',(#7580,#7581,#7582,#7583));
#2351=EDGE_LOOP('',(#7584,#7585,#7586,#7587));
#2352=EDGE_LOOP('',(#7588,#7589,#7590,#7591,#7592,#7593));
#2353=EDGE_LOOP('',(#7594));
#2354=EDGE_LOOP('',(#7595,#7596,#7597,#7598,#7599,#7600));
#2355=EDGE_LOOP('',(#7601,#7602,#7603,#7604));
#2356=EDGE_LOOP('',(#7605,#7606,#7607,#7608));
#2357=EDGE_LOOP('',(#7609,#7610,#7611,#7612));
#2358=EDGE_LOOP('',(#7613));
#2359=EDGE_LOOP('',(#7614,#7615,#7616,#7617));
#2360=EDGE_LOOP('',(#7618,#7619,#7620,#7621));
#2361=EDGE_LOOP('',(#7622,#7623,#7624,#7625));
#2362=EDGE_LOOP('',(#7626,#7627,#7628,#7629));
#2363=EDGE_LOOP('',(#7630));
#2364=EDGE_LOOP('',(#7631));
#2365=EDGE_LOOP('',(#7632,#7633,#7634,#7635));
#2366=EDGE_LOOP('',(#7636,#7637,#7638,#7639));
#2367=EDGE_LOOP('',(#7640,#7641,#7642,#7643));
#2368=EDGE_LOOP('',(#7644,#7645,#7646,#7647));
#2369=EDGE_LOOP('',(#7648));
#2370=EDGE_LOOP('',(#7649));
#2371=EDGE_LOOP('',(#7650,#7651,#7652,#7653));
#2372=EDGE_LOOP('',(#7654,#7655,#7656,#7657));
#2373=EDGE_LOOP('',(#7658));
#2374=EDGE_LOOP('',(#7659));
#2375=EDGE_LOOP('',(#7660));
#2376=EDGE_LOOP('',(#7661));
#2377=EDGE_LOOP('',(#7662,#7663,#7664,#7665));
#2378=EDGE_LOOP('',(#7666,#7667,#7668,#7669));
#2379=EDGE_LOOP('',(#7670));
#2380=EDGE_LOOP('',(#7671));
#2381=EDGE_LOOP('',(#7672));
#2382=EDGE_LOOP('',(#7673));
#2383=EDGE_LOOP('',(#7674,#7675,#7676,#7677));
#2384=EDGE_LOOP('',(#7678,#7679,#7680,#7681));
#2385=EDGE_LOOP('',(#7682));
#2386=EDGE_LOOP('',(#7683));
#2387=EDGE_LOOP('',(#7684));
#2388=EDGE_LOOP('',(#7685));
#2389=EDGE_LOOP('',(#7686,#7687,#7688,#7689));
#2390=EDGE_LOOP('',(#7690,#7691,#7692,#7693));
#2391=EDGE_LOOP('',(#7694));
#2392=EDGE_LOOP('',(#7695));
#2393=EDGE_LOOP('',(#7696));
#2394=EDGE_LOOP('',(#7697));
#2395=EDGE_LOOP('',(#7698,#7699,#7700,#7701,#7702,#7703));
#2396=EDGE_LOOP('',(#7704,#7705,#7706,#7707,#7708));
#2397=EDGE_LOOP('',(#7709,#7710,#7711,#7712));
#2398=EDGE_LOOP('',(#7713,#7714,#7715,#7716));
#2399=EDGE_LOOP('',(#7717));
#2400=EDGE_LOOP('',(#7718));
#2401=EDGE_LOOP('',(#7719,#7720,#7721,#7722,#7723));
#2402=EDGE_LOOP('',(#7724));
#2403=EDGE_LOOP('',(#7725));
#2404=EDGE_LOOP('',(#7726,#7727,#7728,#7729));
#2405=EDGE_LOOP('',(#7730,#7731,#7732,#7733,#7734,#7735));
#2406=EDGE_LOOP('',(#7736,#7737,#7738,#7739,#7740));
#2407=EDGE_LOOP('',(#7741));
#2408=EDGE_LOOP('',(#7742));
#2409=EDGE_LOOP('',(#7743,#7744,#7745,#7746));
#2410=EDGE_LOOP('',(#7747,#7748,#7749,#7750));
#2411=EDGE_LOOP('',(#7751,#7752,#7753,#7754));
#2412=EDGE_LOOP('',(#7755));
#2413=EDGE_LOOP('',(#7756));
#2414=EDGE_LOOP('',(#7757,#7758,#7759,#7760,#7761));
#2415=EDGE_LOOP('',(#7762,#7763));
#2416=EDGE_LOOP('',(#7764,#7765));
#2417=EDGE_LOOP('',(#7766,#7767));
#2418=EDGE_LOOP('',(#7768,#7769));
#2419=EDGE_LOOP('',(#7770,#7771));
#2420=EDGE_LOOP('',(#7772,#7773));
#2421=EDGE_LOOP('',(#7774,#7775));
#2422=EDGE_LOOP('',(#7776,#7777));
#2423=EDGE_LOOP('',(#7778,#7779,#7780,#7781));
#2424=EDGE_LOOP('',(#7782,#7783,#7784,#7785,#7786,#7787,#7788,#7789,#7790,
#7791,#7792,#7793,#7794,#7795,#7796,#7797,#7798,#7799,#7800,#7801));
#2425=EDGE_LOOP('',(#7802,#7803,#7804,#7805));
#2426=EDGE_LOOP('',(#7806,#7807,#7808,#7809));
#2427=EDGE_LOOP('',(#7810,#7811,#7812,#7813));
#2428=EDGE_LOOP('',(#7814,#7815,#7816,#7817));
#2429=EDGE_LOOP('',(#7818,#7819,#7820,#7821));
#2430=EDGE_LOOP('',(#7822,#7823,#7824,#7825,#7826,#7827));
#2431=EDGE_LOOP('',(#7828,#7829,#7830,#7831));
#2432=EDGE_LOOP('',(#7832,#7833,#7834,#7835));
#2433=EDGE_LOOP('',(#7836,#7837,#7838,#7839));
#2434=EDGE_LOOP('',(#7840,#7841,#7842,#7843));
#2435=EDGE_LOOP('',(#7844,#7845,#7846,#7847));
#2436=EDGE_LOOP('',(#7848,#7849,#7850,#7851));
#2437=EDGE_LOOP('',(#7852,#7853,#7854,#7855,#7856,#7857,#7858,#7859,#7860,
#7861,#7862,#7863,#7864,#7865,#7866,#7867,#7868,#7869,#7870,#7871));
#2438=EDGE_LOOP('',(#7872,#7873,#7874,#7875));
#2439=EDGE_LOOP('',(#7876,#7877,#7878,#7879));
#2440=EDGE_LOOP('',(#7880));
#2441=EDGE_LOOP('',(#7881));
#2442=EDGE_LOOP('',(#7882,#7883,#7884,#7885));
#2443=EDGE_LOOP('',(#7886));
#2444=EDGE_LOOP('',(#7887));
#2445=EDGE_LOOP('',(#7888,#7889,#7890,#7891));
#2446=EDGE_LOOP('',(#7892));
#2447=EDGE_LOOP('',(#7893));
#2448=EDGE_LOOP('',(#7894,#7895,#7896,#7897));
#2449=EDGE_LOOP('',(#7898));
#2450=EDGE_LOOP('',(#7899));
#2451=EDGE_LOOP('',(#7900,#7901,#7902,#7903));
#2452=EDGE_LOOP('',(#7904));
#2453=EDGE_LOOP('',(#7905));
#2454=EDGE_LOOP('',(#7906,#7907,#7908,#7909));
#2455=EDGE_LOOP('',(#7910,#7911,#7912,#7913));
#2456=EDGE_LOOP('',(#7914,#7915,#7916,#7917));
#2457=EDGE_LOOP('',(#7918));
#2458=EDGE_LOOP('',(#7919,#7920,#7921,#7922));
#2459=EDGE_LOOP('',(#7923,#7924,#7925,#7926));
#2460=EDGE_LOOP('',(#7927,#7928,#7929,#7930));
#2461=EDGE_LOOP('',(#7931,#7932,#7933,#7934));
#2462=EDGE_LOOP('',(#7935));
#2463=EDGE_LOOP('',(#7936,#7937,#7938,#7939));
#2464=EDGE_LOOP('',(#7940,#7941,#7942,#7943));
#2465=EDGE_LOOP('',(#7944,#7945,#7946,#7947));
#2466=EDGE_LOOP('',(#7948,#7949,#7950,#7951));
#2467=EDGE_LOOP('',(#7952,#7953,#7954,#7955));
#2468=EDGE_LOOP('',(#7956,#7957,#7958,#7959));
#2469=EDGE_LOOP('',(#7960,#7961,#7962,#7963));
#2470=EDGE_LOOP('',(#7964,#7965,#7966,#7967));
#2471=EDGE_LOOP('',(#7968));
#2472=EDGE_LOOP('',(#7969));
#2473=EDGE_LOOP('',(#7970));
#2474=EDGE_LOOP('',(#7971));
#2475=EDGE_LOOP('',(#7972));
#2476=EDGE_LOOP('',(#7973));
#2477=EDGE_LOOP('',(#7974,#7975,#7976,#7977));
#2478=EDGE_LOOP('',(#7978,#7979,#7980,#7981));
#2479=EDGE_LOOP('',(#7982));
#2480=EDGE_LOOP('',(#7983));
#2481=EDGE_LOOP('',(#7984));
#2482=EDGE_LOOP('',(#7985));
#2483=EDGE_LOOP('',(#7986));
#2484=EDGE_LOOP('',(#7987));
#2485=EDGE_LOOP('',(#7988,#7989,#7990,#7991));
#2486=EDGE_LOOP('',(#7992,#7993,#7994,#7995));
#2487=EDGE_LOOP('',(#7996,#7997,#7998,#7999));
#2488=EDGE_LOOP('',(#8000,#8001,#8002,#8003));
#2489=EDGE_LOOP('',(#8004,#8005,#8006,#8007));
#2490=EDGE_LOOP('',(#8008,#8009,#8010,#8011));
#2491=EDGE_LOOP('',(#8012,#8013,#8014,#8015));
#2492=EDGE_LOOP('',(#8016,#8017,#8018,#8019));
#2493=EDGE_LOOP('',(#8020,#8021,#8022,#8023));
#2494=EDGE_LOOP('',(#8024,#8025,#8026,#8027));
#2495=EDGE_LOOP('',(#8028,#8029,#8030,#8031));
#2496=EDGE_LOOP('',(#8032));
#2497=EDGE_LOOP('',(#8033));
#2498=EDGE_LOOP('',(#8034));
#2499=EDGE_LOOP('',(#8035));
#2500=EDGE_LOOP('',(#8036));
#2501=EDGE_LOOP('',(#8037));
#2502=EDGE_LOOP('',(#8038,#8039,#8040,#8041));
#2503=EDGE_LOOP('',(#8042,#8043,#8044,#8045));
#2504=EDGE_LOOP('',(#8046));
#2505=EDGE_LOOP('',(#8047));
#2506=EDGE_LOOP('',(#8048));
#2507=EDGE_LOOP('',(#8049));
#2508=EDGE_LOOP('',(#8050));
#2509=EDGE_LOOP('',(#8051));
#2510=EDGE_LOOP('',(#8052,#8053,#8054,#8055));
#2511=EDGE_LOOP('',(#8056,#8057,#8058,#8059));
#2512=EDGE_LOOP('',(#8060,#8061,#8062,#8063));
#2513=EDGE_LOOP('',(#8064,#8065,#8066,#8067));
#2514=EDGE_LOOP('',(#8068,#8069,#8070,#8071));
#2515=EDGE_LOOP('',(#8072,#8073,#8074,#8075));
#2516=EDGE_LOOP('',(#8076,#8077,#8078,#8079));
#2517=EDGE_LOOP('',(#8080,#8081,#8082,#8083));
#2518=EDGE_LOOP('',(#8084,#8085,#8086,#8087));
#2519=EDGE_LOOP('',(#8088,#8089,#8090,#8091));
#2520=EDGE_LOOP('',(#8092));
#2521=EDGE_LOOP('',(#8093));
#2522=EDGE_LOOP('',(#8094));
#2523=EDGE_LOOP('',(#8095));
#2524=EDGE_LOOP('',(#8096));
#2525=EDGE_LOOP('',(#8097));
#2526=EDGE_LOOP('',(#8098,#8099,#8100,#8101));
#2527=EDGE_LOOP('',(#8102,#8103,#8104,#8105));
#2528=EDGE_LOOP('',(#8106));
#2529=EDGE_LOOP('',(#8107));
#2530=EDGE_LOOP('',(#8108));
#2531=EDGE_LOOP('',(#8109));
#2532=EDGE_LOOP('',(#8110));
#2533=EDGE_LOOP('',(#8111));
#2534=EDGE_LOOP('',(#8112,#8113,#8114,#8115));
#2535=EDGE_LOOP('',(#8116,#8117,#8118,#8119));
#2536=EDGE_LOOP('',(#8120,#8121,#8122,#8123));
#2537=EDGE_LOOP('',(#8124));
#2538=EDGE_LOOP('',(#8125));
#2539=EDGE_LOOP('',(#8126));
#2540=EDGE_LOOP('',(#8127,#8128,#8129,#8130));
#2541=EDGE_LOOP('',(#8131));
#2542=EDGE_LOOP('',(#8132,#8133,#8134,#8135));
#2543=EDGE_LOOP('',(#8136));
#2544=EDGE_LOOP('',(#8137));
#2545=EDGE_LOOP('',(#8138,#8139,#8140,#8141));
#2546=EDGE_LOOP('',(#8142,#8143,#8144,#8145));
#2547=EDGE_LOOP('',(#8146));
#2548=EDGE_LOOP('',(#8147));
#2549=EDGE_LOOP('',(#8148));
#2550=EDGE_LOOP('',(#8149));
#2551=EDGE_LOOP('',(#8150,#8151,#8152,#8153));
#2552=EDGE_LOOP('',(#8154,#8155,#8156,#8157));
#2553=EDGE_LOOP('',(#8158));
#2554=EDGE_LOOP('',(#8159));
#2555=EDGE_LOOP('',(#8160));
#2556=EDGE_LOOP('',(#8161));
#2557=EDGE_LOOP('',(#8162,#8163,#8164,#8165));
#2558=EDGE_LOOP('',(#8166,#8167,#8168,#8169));
#2559=EDGE_LOOP('',(#8170));
#2560=EDGE_LOOP('',(#8171));
#2561=EDGE_LOOP('',(#8172));
#2562=EDGE_LOOP('',(#8173));
#2563=EDGE_LOOP('',(#8174,#8175,#8176,#8177));
#2564=EDGE_LOOP('',(#8178,#8179,#8180,#8181));
#2565=EDGE_LOOP('',(#8182,#8183,#8184,#8185));
#2566=EDGE_LOOP('',(#8186,#8187,#8188,#8189));
#2567=EDGE_LOOP('',(#8190,#8191,#8192,#8193));
#2568=EDGE_LOOP('',(#8194));
#2569=EDGE_LOOP('',(#8195));
#2570=EDGE_LOOP('',(#8196,#8197,#8198,#8199));
#2571=EDGE_LOOP('',(#8200));
#2572=EDGE_LOOP('',(#8201));
#2573=EDGE_LOOP('',(#8202,#8203,#8204,#8205));
#2574=EDGE_LOOP('',(#8206));
#2575=EDGE_LOOP('',(#8207));
#2576=EDGE_LOOP('',(#8208,#8209,#8210,#8211));
#2577=EDGE_LOOP('',(#8212));
#2578=EDGE_LOOP('',(#8213));
#2579=EDGE_LOOP('',(#8214,#8215,#8216,#8217));
#2580=EDGE_LOOP('',(#8218));
#2581=EDGE_LOOP('',(#8219));
#2582=EDGE_LOOP('',(#8220,#8221,#8222,#8223));
#2583=EDGE_LOOP('',(#8224));
#2584=EDGE_LOOP('',(#8225));
#2585=EDGE_LOOP('',(#8226,#8227,#8228,#8229));
#2586=EDGE_LOOP('',(#8230,#8231,#8232,#8233));
#2587=EDGE_LOOP('',(#8234,#8235,#8236,#8237));
#2588=EDGE_LOOP('',(#8238,#8239,#8240,#8241));
#2589=EDGE_LOOP('',(#8242,#8243,#8244,#8245));
#2590=EDGE_LOOP('',(#8246,#8247,#8248,#8249));
#2591=EDGE_LOOP('',(#8250));
#2592=EDGE_LOOP('',(#8251));
#2593=EDGE_LOOP('',(#8252,#8253,#8254,#8255));
#2594=EDGE_LOOP('',(#8256,#8257,#8258,#8259));
#2595=EDGE_LOOP('',(#8260));
#2596=EDGE_LOOP('',(#8261));
#2597=EDGE_LOOP('',(#8262,#8263,#8264,#8265));
#2598=EDGE_LOOP('',(#8266,#8267,#8268,#8269));
#2599=EDGE_LOOP('',(#8270,#8271,#8272,#8273));
#2600=EDGE_LOOP('',(#8274,#8275,#8276,#8277));
#2601=EDGE_LOOP('',(#8278,#8279,#8280,#8281));
#2602=EDGE_LOOP('',(#8282,#8283,#8284,#8285));
#2603=EDGE_LOOP('',(#8286,#8287,#8288,#8289));
#2604=EDGE_LOOP('',(#8290,#8291,#8292,#8293));
#2605=EDGE_LOOP('',(#8294,#8295,#8296,#8297,#8298,#8299));
#2606=EDGE_LOOP('',(#8300,#8301,#8302,#8303,#8304,#8305));
#2607=EDGE_LOOP('',(#8306));
#2608=EDGE_LOOP('',(#8307));
#2609=EDGE_LOOP('',(#8308,#8309,#8310,#8311));
#2610=EDGE_LOOP('',(#8312,#8313,#8314,#8315));
#2611=EDGE_LOOP('',(#8316,#8317,#8318,#8319));
#2612=EDGE_LOOP('',(#8320));
#2613=EDGE_LOOP('',(#8321));
#2614=EDGE_LOOP('',(#8322,#8323,#8324,#8325));
#2615=EDGE_LOOP('',(#8326,#8327,#8328,#8329));
#2616=LINE('',#13738,#3227);
#2617=LINE('',#13744,#3228);
#2618=LINE('',#13750,#3229);
#2619=LINE('',#13756,#3230);
#2620=LINE('',#13762,#3231);
#2621=LINE('',#13768,#3232);
#2622=LINE('',#13774,#3233);
#2623=LINE('',#13780,#3234);
#2624=LINE('',#13786,#3235);
#2625=LINE('',#13792,#3236);
#2626=LINE('',#13798,#3237);
#2627=LINE('',#13804,#3238);
#2628=LINE('',#13809,#3239);
#2629=LINE('',#13811,#3240);
#2630=LINE('',#13813,#3241);
#2631=LINE('',#13814,#3242);
#2632=LINE('',#13817,#3243);
#2633=LINE('',#13819,#3244);
#2634=LINE('',#13820,#3245);
#2635=LINE('',#13823,#3246);
#2636=LINE('',#13825,#3247);
#2637=LINE('',#13826,#3248);
#2638=LINE('',#13828,#3249);
#2639=LINE('',#13829,#3250);
#2640=LINE('',#13837,#3251);
#2641=LINE('',#13844,#3252);
#2642=LINE('',#13851,#3253);
#2643=LINE('',#13860,#3254);
#2644=LINE('',#13869,#3255);
#2645=LINE('',#13878,#3256);
#2646=LINE('',#13886,#3257);
#2647=LINE('',#13890,#3258);
#2648=LINE('',#13894,#3259);
#2649=LINE('',#13898,#3260);
#2650=LINE('',#13902,#3261);
#2651=LINE('',#13904,#3262);
#2652=LINE('',#13906,#3263);
#2653=LINE('',#13907,#3264);
#2654=LINE('',#13910,#3265);
#2655=LINE('',#13912,#3266);
#2656=LINE('',#13913,#3267);
#2657=LINE('',#13916,#3268);
#2658=LINE('',#13918,#3269);
#2659=LINE('',#13919,#3270);
#2660=LINE('',#13921,#3271);
#2661=LINE('',#13922,#3272);
#2662=LINE('',#13930,#3273);
#2663=LINE('',#13936,#3274);
#2664=LINE('',#13945,#3275);
#2665=LINE('',#13951,#3276);
#2666=LINE('',#13960,#3277);
#2667=LINE('',#13967,#3278);
#2668=LINE('',#13974,#3279);
#2669=LINE('',#13983,#3280);
#2670=LINE('',#13992,#3281);
#2671=LINE('',#14001,#3282);
#2672=LINE('',#14009,#3283);
#2673=LINE('',#14013,#3284);
#2674=LINE('',#14017,#3285);
#2675=LINE('',#14021,#3286);
#2676=LINE('',#14025,#3287);
#2677=LINE('',#14027,#3288);
#2678=LINE('',#14029,#3289);
#2679=LINE('',#14030,#3290);
#2680=LINE('',#14033,#3291);
#2681=LINE('',#14035,#3292);
#2682=LINE('',#14036,#3293);
#2683=LINE('',#14039,#3294);
#2684=LINE('',#14041,#3295);
#2685=LINE('',#14042,#3296);
#2686=LINE('',#14044,#3297);
#2687=LINE('',#14045,#3298);
#2688=LINE('',#14053,#3299);
#2689=LINE('',#14059,#3300);
#2690=LINE('',#14068,#3301);
#2691=LINE('',#14074,#3302);
#2692=LINE('',#14082,#3303);
#2693=LINE('',#14086,#3304);
#2694=LINE('',#14092,#3305);
#2695=LINE('',#14094,#3306);
#2696=LINE('',#14100,#3307);
#2697=LINE('',#14107,#3308);
#2698=LINE('',#14109,#3309);
#2699=LINE('',#14111,#3310);
#2700=LINE('',#14112,#3311);
#2701=LINE('',#14114,#3312);
#2702=LINE('',#14115,#3313);
#2703=LINE('',#14127,#3314);
#2704=LINE('',#14131,#3315);
#2705=LINE('',#14135,#3316);
#2706=LINE('',#14140,#3317);
#2707=LINE('',#14145,#3318);
#2708=LINE('',#14150,#3319);
#2709=LINE('',#14155,#3320);
#2710=LINE('',#14156,#3321);
#2711=LINE('',#14157,#3322);
#2712=LINE('',#14160,#3323);
#2713=LINE('',#14161,#3324);
#2714=LINE('',#14164,#3325);
#2715=LINE('',#14165,#3326);
#2716=LINE('',#14167,#3327);
#2717=LINE('',#14173,#3328);
#2718=LINE('',#14177,#3329);
#2719=LINE('',#14183,#3330);
#2720=LINE('',#14185,#3331);
#2721=LINE('',#14191,#3332);
#2722=LINE('',#14198,#3333);
#2723=LINE('',#14200,#3334);
#2724=LINE('',#14202,#3335);
#2725=LINE('',#14203,#3336);
#2726=LINE('',#14205,#3337);
#2727=LINE('',#14206,#3338);
#2728=LINE('',#14218,#3339);
#2729=LINE('',#14222,#3340);
#2730=LINE('',#14226,#3341);
#2731=LINE('',#14231,#3342);
#2732=LINE('',#14236,#3343);
#2733=LINE('',#14241,#3344);
#2734=LINE('',#14246,#3345);
#2735=LINE('',#14247,#3346);
#2736=LINE('',#14248,#3347);
#2737=LINE('',#14251,#3348);
#2738=LINE('',#14252,#3349);
#2739=LINE('',#14255,#3350);
#2740=LINE('',#14256,#3351);
#2741=LINE('',#14258,#3352);
#2742=LINE('',#14264,#3353);
#2743=LINE('',#14266,#3354);
#2744=LINE('',#14268,#3355);
#2745=LINE('',#14269,#3356);
#2746=LINE('',#14272,#3357);
#2747=LINE('',#14274,#3358);
#2748=LINE('',#14275,#3359);
#2749=LINE('',#14278,#3360);
#2750=LINE('',#14280,#3361);
#2751=LINE('',#14281,#3362);
#2752=LINE('',#14283,#3363);
#2753=LINE('',#14284,#3364);
#2754=LINE('',#14291,#3365);
#2755=LINE('',#14293,#3366);
#2756=LINE('',#14295,#3367);
#2757=LINE('',#14296,#3368);
#2758=LINE('',#14299,#3369);
#2759=LINE('',#14301,#3370);
#2760=LINE('',#14302,#3371);
#2761=LINE('',#14305,#3372);
#2762=LINE('',#14307,#3373);
#2763=LINE('',#14308,#3374);
#2764=LINE('',#14310,#3375);
#2765=LINE('',#14311,#3376);
#2766=LINE('',#14321,#3377);
#2767=LINE('',#14325,#3378);
#2768=LINE('',#14329,#3379);
#2769=LINE('',#14336,#3380);
#2770=LINE('',#14340,#3381);
#2771=LINE('',#14344,#3382);
#2772=LINE('',#14349,#3383);
#2773=LINE('',#14351,#3384);
#2774=LINE('',#14353,#3385);
#2775=LINE('',#14354,#3386);
#2776=LINE('',#14357,#3387);
#2777=LINE('',#14359,#3388);
#2778=LINE('',#14360,#3389);
#2779=LINE('',#14363,#3390);
#2780=LINE('',#14365,#3391);
#2781=LINE('',#14366,#3392);
#2782=LINE('',#14369,#3393);
#2783=LINE('',#14371,#3394);
#2784=LINE('',#14372,#3395);
#2785=LINE('',#14375,#3396);
#2786=LINE('',#14377,#3397);
#2787=LINE('',#14378,#3398);
#2788=LINE('',#14380,#3399);
#2789=LINE('',#14381,#3400);
#2790=LINE('',#14390,#3401);
#2791=LINE('',#14396,#3402);
#2792=LINE('',#14405,#3403);
#2793=LINE('',#14407,#3404);
#2794=LINE('',#14412,#3405);
#2795=LINE('',#14415,#3406);
#2796=LINE('',#14419,#3407);
#2797=LINE('',#14422,#3408);
#2798=LINE('',#14424,#3409);
#2799=LINE('',#14425,#3410);
#2800=LINE('',#14429,#3411);
#2801=LINE('',#14431,#3412);
#2802=LINE('',#14434,#3413);
#2803=LINE('',#14435,#3414);
#2804=LINE('',#14439,#3415);
#2805=LINE('',#14441,#3416);
#2806=LINE('',#14443,#3417);
#2807=LINE('',#14444,#3418);
#2808=LINE('',#14450,#3419);
#2809=LINE('',#14452,#3420);
#2810=LINE('',#14453,#3421);
#2811=LINE('',#14455,#3422);
#2812=LINE('',#14457,#3423);
#2813=LINE('',#14458,#3424);
#2814=LINE('',#14467,#3425);
#2815=LINE('',#14469,#3426);
#2816=LINE('',#14471,#3427);
#2817=LINE('',#14472,#3428);
#2818=LINE('',#14475,#3429);
#2819=LINE('',#14477,#3430);
#2820=LINE('',#14478,#3431);
#2821=LINE('',#14481,#3432);
#2822=LINE('',#14483,#3433);
#2823=LINE('',#14484,#3434);
#2824=LINE('',#14486,#3435);
#2825=LINE('',#14487,#3436);
#2826=LINE('',#14492,#3437);
#2827=LINE('',#14496,#3438);
#2828=LINE('',#14500,#3439);
#2829=LINE('',#14501,#3440);
#2830=LINE('',#14502,#3441);
#2831=LINE('',#14505,#3442);
#2832=LINE('',#14506,#3443);
#2833=LINE('',#14509,#3444);
#2834=LINE('',#14510,#3445);
#2835=LINE('',#14512,#3446);
#2836=LINE('',#14519,#3447);
#2837=LINE('',#14574,#3448);
#2838=LINE('',#14646,#3449);
#2839=LINE('',#14691,#3450);
#2840=LINE('',#14859,#3451);
#2841=LINE('',#14930,#3452);
#2842=LINE('',#14933,#3453);
#2843=LINE('',#15004,#3454);
#2844=LINE('',#15014,#3455);
#2845=LINE('',#15019,#3456);
#2846=LINE('',#15027,#3457);
#2847=LINE('',#15033,#3458);
#2848=LINE('',#15041,#3459);
#2849=LINE('',#15043,#3460);
#2850=LINE('',#15045,#3461);
#2851=LINE('',#15046,#3462);
#2852=LINE('',#15049,#3463);
#2853=LINE('',#15051,#3464);
#2854=LINE('',#15052,#3465);
#2855=LINE('',#15055,#3466);
#2856=LINE('',#15057,#3467);
#2857=LINE('',#15058,#3468);
#2858=LINE('',#15061,#3469);
#2859=LINE('',#15063,#3470);
#2860=LINE('',#15064,#3471);
#2861=LINE('',#15067,#3472);
#2862=LINE('',#15069,#3473);
#2863=LINE('',#15070,#3474);
#2864=LINE('',#15072,#3475);
#2865=LINE('',#15073,#3476);
#2866=LINE('',#15085,#3477);
#2867=LINE('',#15089,#3478);
#2868=LINE('',#15093,#3479);
#2869=LINE('',#15100,#3480);
#2870=LINE('',#15102,#3481);
#2871=LINE('',#15107,#3482);
#2872=LINE('',#15111,#3483);
#2873=LINE('',#15114,#3484);
#2874=LINE('',#15118,#3485);
#2875=LINE('',#15122,#3486);
#2876=LINE('',#15125,#3487);
#2877=LINE('',#15128,#3488);
#2878=LINE('',#15130,#3489);
#2879=LINE('',#15132,#3490);
#2880=LINE('',#15134,#3491);
#2881=LINE('',#15135,#3492);
#2882=LINE('',#15140,#3493);
#2883=LINE('',#15142,#3494);
#2884=LINE('',#15143,#3495);
#2885=LINE('',#15149,#3496);
#2886=LINE('',#15151,#3497);
#2887=LINE('',#15152,#3498);
#2888=LINE('',#15154,#3499);
#2889=LINE('',#15155,#3500);
#2890=LINE('',#15162,#3501);
#2891=LINE('',#15166,#3502);
#2892=LINE('',#15171,#3503);
#2893=LINE('',#15175,#3504);
#2894=LINE('',#15180,#3505);
#2895=LINE('',#15184,#3506);
#2896=LINE('',#15186,#3507);
#2897=LINE('',#15187,#3508);
#2898=LINE('',#15189,#3509);
#2899=LINE('',#15191,#3510);
#2900=LINE('',#15193,#3511);
#2901=LINE('',#15195,#3512);
#2902=LINE('',#15197,#3513);
#2903=LINE('',#15198,#3514);
#2904=LINE('',#15201,#3515);
#2905=LINE('',#15202,#3516);
#2906=LINE('',#15205,#3517);
#2907=LINE('',#15206,#3518);
#2908=LINE('',#15208,#3519);
#2909=LINE('',#15211,#3520);
#2910=LINE('',#15212,#3521);
#2911=LINE('',#15215,#3522);
#2912=LINE('',#15216,#3523);
#2913=LINE('',#15219,#3524);
#2914=LINE('',#15220,#3525);
#2915=LINE('',#15223,#3526);
#2916=LINE('',#15224,#3527);
#2917=LINE('',#15227,#3528);
#2918=LINE('',#15228,#3529);
#2919=LINE('',#15230,#3530);
#2920=LINE('',#15237,#3531);
#2921=LINE('',#15241,#3532);
#2922=LINE('',#15248,#3533);
#2923=LINE('',#15255,#3534);
#2924=LINE('',#15257,#3535);
#2925=LINE('',#15259,#3536);
#2926=LINE('',#15260,#3537);
#2927=LINE('',#15263,#3538);
#2928=LINE('',#15265,#3539);
#2929=LINE('',#15266,#3540);
#2930=LINE('',#15269,#3541);
#2931=LINE('',#15271,#3542);
#2932=LINE('',#15272,#3543);
#2933=LINE('',#15275,#3544);
#2934=LINE('',#15277,#3545);
#2935=LINE('',#15278,#3546);
#2936=LINE('',#15281,#3547);
#2937=LINE('',#15283,#3548);
#2938=LINE('',#15284,#3549);
#2939=LINE('',#15286,#3550);
#2940=LINE('',#15287,#3551);
#2941=LINE('',#15299,#3552);
#2942=LINE('',#15303,#3553);
#2943=LINE('',#15307,#3554);
#2944=LINE('',#15314,#3555);
#2945=LINE('',#15316,#3556);
#2946=LINE('',#15324,#3557);
#2947=LINE('',#15328,#3558);
#2948=LINE('',#15332,#3559);
#2949=LINE('',#15339,#3560);
#2950=LINE('',#15343,#3561);
#2951=LINE('',#15347,#3562);
#2952=LINE('',#15352,#3563);
#2953=LINE('',#15354,#3564);
#2954=LINE('',#15356,#3565);
#2955=LINE('',#15357,#3566);
#2956=LINE('',#15360,#3567);
#2957=LINE('',#15362,#3568);
#2958=LINE('',#15363,#3569);
#2959=LINE('',#15366,#3570);
#2960=LINE('',#15368,#3571);
#2961=LINE('',#15369,#3572);
#2962=LINE('',#15372,#3573);
#2963=LINE('',#15374,#3574);
#2964=LINE('',#15375,#3575);
#2965=LINE('',#15378,#3576);
#2966=LINE('',#15380,#3577);
#2967=LINE('',#15381,#3578);
#2968=LINE('',#15383,#3579);
#2969=LINE('',#15384,#3580);
#2970=LINE('',#15395,#3581);
#2971=LINE('',#15398,#3582);
#2972=LINE('',#15405,#3583);
#2973=LINE('',#15407,#3584);
#2974=LINE('',#15409,#3585);
#2975=LINE('',#15410,#3586);
#2976=LINE('',#15415,#3587);
#2977=LINE('',#15416,#3588);
#2978=LINE('',#15419,#3589);
#2979=LINE('',#15421,#3590);
#2980=LINE('',#15422,#3591);
#2981=LINE('',#15424,#3592);
#2982=LINE('',#15429,#3593);
#2983=LINE('',#15438,#3594);
#2984=LINE('',#15459,#3595);
#2985=LINE('',#15514,#3596);
#2986=LINE('',#15519,#3597);
#2987=LINE('',#15525,#3598);
#2988=LINE('',#15533,#3599);
#2989=LINE('',#15554,#3600);
#2990=LINE('',#15609,#3601);
#2991=LINE('',#15614,#3602);
#2992=LINE('',#15620,#3603);
#2993=LINE('',#15629,#3604);
#2994=LINE('',#15635,#3605);
#2995=LINE('',#15643,#3606);
#2996=LINE('',#15647,#3607);
#2997=LINE('',#15653,#3608);
#2998=LINE('',#15655,#3609);
#2999=LINE('',#15657,#3610);
#3000=LINE('',#15663,#3611);
#3001=LINE('',#15669,#3612);
#3002=LINE('',#15693,#3613);
#3003=LINE('',#15731,#3614);
#3004=LINE('',#15739,#3615);
#3005=LINE('',#15743,#3616);
#3006=LINE('',#15745,#3617);
#3007=LINE('',#15749,#3618);
#3008=LINE('',#15750,#3619);
#3009=LINE('',#15753,#3620);
#3010=LINE('',#15754,#3621);
#3011=LINE('',#15756,#3622);
#3012=LINE('',#15767,#3623);
#3013=LINE('',#15770,#3624);
#3014=LINE('',#15780,#3625);
#3015=LINE('',#15791,#3626);
#3016=LINE('',#15795,#3627);
#3017=LINE('',#15803,#3628);
#3018=LINE('',#15809,#3629);
#3019=LINE('',#15818,#3630);
#3020=LINE('',#15824,#3631);
#3021=LINE('',#15833,#3632);
#3022=LINE('',#15839,#3633);
#3023=LINE('',#15847,#3634);
#3024=LINE('',#15849,#3635);
#3025=LINE('',#15851,#3636);
#3026=LINE('',#15853,#3637);
#3027=LINE('',#15855,#3638);
#3028=LINE('',#15857,#3639);
#3029=LINE('',#15859,#3640);
#3030=LINE('',#15860,#3641);
#3031=LINE('',#15863,#3642);
#3032=LINE('',#15865,#3643);
#3033=LINE('',#15866,#3644);
#3034=LINE('',#15869,#3645);
#3035=LINE('',#15870,#3646);
#3036=LINE('',#15873,#3647);
#3037=LINE('',#15874,#3648);
#3038=LINE('',#15877,#3649);
#3039=LINE('',#15878,#3650);
#3040=LINE('',#15882,#3651);
#3041=LINE('',#15883,#3652);
#3042=LINE('',#15885,#3653);
#3043=LINE('',#15886,#3654);
#3044=LINE('',#15888,#3655);
#3045=LINE('',#15890,#3656);
#3046=LINE('',#15892,#3657);
#3047=LINE('',#15898,#3658);
#3048=LINE('',#15900,#3659);
#3049=LINE('',#15902,#3660);
#3050=LINE('',#15903,#3661);
#3051=LINE('',#15906,#3662);
#3052=LINE('',#15908,#3663);
#3053=LINE('',#15909,#3664);
#3054=LINE('',#15912,#3665);
#3055=LINE('',#15914,#3666);
#3056=LINE('',#15915,#3667);
#3057=LINE('',#15918,#3668);
#3058=LINE('',#15920,#3669);
#3059=LINE('',#15921,#3670);
#3060=LINE('',#15924,#3671);
#3061=LINE('',#15926,#3672);
#3062=LINE('',#15927,#3673);
#3063=LINE('',#15929,#3674);
#3064=LINE('',#15930,#3675);
#3065=LINE('',#15938,#3676);
#3066=LINE('',#15942,#3677);
#3067=LINE('',#15946,#3678);
#3068=LINE('',#15954,#3679);
#3069=LINE('',#15960,#3680);
#3070=LINE('',#15965,#3681);
#3071=LINE('',#15969,#3682);
#3072=LINE('',#15973,#3683);
#3073=LINE('',#15976,#3684);
#3074=LINE('',#15979,#3685);
#3075=LINE('',#15980,#3686);
#3076=LINE('',#15983,#3687);
#3077=LINE('',#15986,#3688);
#3078=LINE('',#15993,#3689);
#3079=LINE('',#15999,#3690);
#3080=LINE('',#16008,#3691);
#3081=LINE('',#16014,#3692);
#3082=LINE('',#16023,#3693);
#3083=LINE('',#16029,#3694);
#3084=LINE('',#16038,#3695);
#3085=LINE('',#16044,#3696);
#3086=LINE('',#16062,#3697);
#3087=LINE('',#16068,#3698);
#3088=LINE('',#16072,#3699);
#3089=LINE('',#16078,#3700);
#3090=LINE('',#16083,#3701);
#3091=LINE('',#16098,#3702);
#3092=LINE('',#16107,#3703);
#3093=LINE('',#16111,#3704);
#3094=LINE('',#16115,#3705);
#3095=LINE('',#16118,#3706);
#3096=LINE('',#16271,#3707);
#3097=LINE('',#16567,#3708);
#3098=LINE('',#16609,#3709);
#3099=LINE('',#16614,#3710);
#3100=LINE('',#16623,#3711);
#3101=LINE('',#16628,#3712);
#3102=LINE('',#16647,#3713);
#3103=LINE('',#16652,#3714);
#3104=LINE('',#16654,#3715);
#3105=LINE('',#16656,#3716);
#3106=LINE('',#16657,#3717);
#3107=LINE('',#16660,#3718);
#3108=LINE('',#16662,#3719);
#3109=LINE('',#16663,#3720);
#3110=LINE('',#16666,#3721);
#3111=LINE('',#16668,#3722);
#3112=LINE('',#16669,#3723);
#3113=LINE('',#16671,#3724);
#3114=LINE('',#16673,#3725);
#3115=LINE('',#16678,#3726);
#3116=LINE('',#16684,#3727);
#3117=LINE('',#16690,#3728);
#3118=LINE('',#16696,#3729);
#3119=LINE('',#16702,#3730);
#3120=LINE('',#16708,#3731);
#3121=LINE('',#16713,#3732);
#3122=LINE('',#16715,#3733);
#3123=LINE('',#16717,#3734);
#3124=LINE('',#16718,#3735);
#3125=LINE('',#16721,#3736);
#3126=LINE('',#16723,#3737);
#3127=LINE('',#16724,#3738);
#3128=LINE('',#16727,#3739);
#3129=LINE('',#16729,#3740);
#3130=LINE('',#16730,#3741);
#3131=LINE('',#16732,#3742);
#3132=LINE('',#16733,#3743);
#3133=LINE('',#16741,#3744);
#3134=LINE('',#16747,#3745);
#3135=LINE('',#16753,#3746);
#3136=LINE('',#16759,#3747);
#3137=LINE('',#16765,#3748);
#3138=LINE('',#16771,#3749);
#3139=LINE('',#16776,#3750);
#3140=LINE('',#16778,#3751);
#3141=LINE('',#16780,#3752);
#3142=LINE('',#16781,#3753);
#3143=LINE('',#16784,#3754);
#3144=LINE('',#16786,#3755);
#3145=LINE('',#16787,#3756);
#3146=LINE('',#16790,#3757);
#3147=LINE('',#16792,#3758);
#3148=LINE('',#16793,#3759);
#3149=LINE('',#16795,#3760);
#3150=LINE('',#16796,#3761);
#3151=LINE('',#16804,#3762);
#3152=LINE('',#16810,#3763);
#3153=LINE('',#16816,#3764);
#3154=LINE('',#16822,#3765);
#3155=LINE('',#16828,#3766);
#3156=LINE('',#16834,#3767);
#3157=LINE('',#16839,#3768);
#3158=LINE('',#16841,#3769);
#3159=LINE('',#16843,#3770);
#3160=LINE('',#16844,#3771);
#3161=LINE('',#16847,#3772);
#3162=LINE('',#16849,#3773);
#3163=LINE('',#16850,#3774);
#3164=LINE('',#16853,#3775);
#3165=LINE('',#16855,#3776);
#3166=LINE('',#16856,#3777);
#3167=LINE('',#16858,#3778);
#3168=LINE('',#16859,#3779);
#3169=LINE('',#16867,#3780);
#3170=LINE('',#16877,#3781);
#3171=LINE('',#16883,#3782);
#3172=LINE('',#16890,#3783);
#3173=LINE('',#16896,#3784);
#3174=LINE('',#16905,#3785);
#3175=LINE('',#16911,#3786);
#3176=LINE('',#16920,#3787);
#3177=LINE('',#16926,#3788);
#3178=LINE('',#16937,#3789);
#3179=LINE('',#16939,#3790);
#3180=LINE('',#16940,#3791);
#3181=LINE('',#16943,#3792);
#3182=LINE('',#16945,#3793);
#3183=LINE('',#16946,#3794);
#3184=LINE('',#16951,#3795);
#3185=LINE('',#16952,#3796);
#3186=LINE('',#16954,#3797);
#3187=LINE('',#16955,#3798);
#3188=LINE('',#16965,#3799);
#3189=LINE('',#16972,#3800);
#3190=LINE('',#16979,#3801);
#3191=LINE('',#16986,#3802);
#3192=LINE('',#16993,#3803);
#3193=LINE('',#16998,#3804);
#3194=LINE('',#17005,#3805);
#3195=LINE('',#17008,#3806);
#3196=LINE('',#17011,#3807);
#3197=LINE('',#17013,#3808);
#3198=LINE('',#17014,#3809);
#3199=LINE('',#17020,#3810);
#3200=LINE('',#17022,#3811);
#3201=LINE('',#17023,#3812);
#3202=LINE('',#17032,#3813);
#3203=LINE('',#17037,#3814);
#3204=LINE('',#17044,#3815);
#3205=LINE('',#17046,#3816);
#3206=LINE('',#17048,#3817);
#3207=LINE('',#17049,#3818);
#3208=LINE('',#17052,#3819);
#3209=LINE('',#17054,#3820);
#3210=LINE('',#17055,#3821);
#3211=LINE('',#17058,#3822);
#3212=LINE('',#17060,#3823);
#3213=LINE('',#17061,#3824);
#3214=LINE('',#17064,#3825);
#3215=LINE('',#17066,#3826);
#3216=LINE('',#17067,#3827);
#3217=LINE('',#17070,#3828);
#3218=LINE('',#17072,#3829);
#3219=LINE('',#17073,#3830);
#3220=LINE('',#17075,#3831);
#3221=LINE('',#17076,#3832);
#3222=LINE('',#17088,#3833);
#3223=LINE('',#17092,#3834);
#3224=LINE('',#17096,#3835);
#3225=LINE('',#17103,#3836);
#3226=LINE('',#17105,#3837);
#3227=VECTOR('',#10840,0.164999999999999);
#3228=VECTOR('',#10847,0.164999999999999);
#3229=VECTOR('',#10854,0.165);
#3230=VECTOR('',#10861,0.165);
#3231=VECTOR('',#10868,0.21);
#3232=VECTOR('',#10875,0.21);
#3233=VECTOR('',#10882,0.21);
#3234=VECTOR('',#10889,0.21);
#3235=VECTOR('',#10896,0.21);
#3236=VECTOR('',#10903,0.21);
#3237=VECTOR('',#10910,0.21);
#3238=VECTOR('',#10917,0.21);
#3239=VECTOR('',#10922,1.);
#3240=VECTOR('',#10923,1.);
#3241=VECTOR('',#10924,1.);
#3242=VECTOR('',#10925,1.);
#3243=VECTOR('',#10928,1.);
#3244=VECTOR('',#10929,1.);
#3245=VECTOR('',#10930,1.);
#3246=VECTOR('',#10933,1.);
#3247=VECTOR('',#10934,1.);
#3248=VECTOR('',#10935,1.);
#3249=VECTOR('',#10938,1.);
#3250=VECTOR('',#10939,1.);
#3251=VECTOR('',#10950,0.34);
#3252=VECTOR('',#10959,0.34);
#3253=VECTOR('',#10968,0.5);
#3254=VECTOR('',#10979,0.5);
#3255=VECTOR('',#10990,0.5);
#3256=VECTOR('',#11001,0.5);
#3257=VECTOR('',#11012,0.275);
#3258=VECTOR('',#11017,0.275);
#3259=VECTOR('',#11022,0.275);
#3260=VECTOR('',#11027,0.275);
#3261=VECTOR('',#11030,1.);
#3262=VECTOR('',#11031,1.);
#3263=VECTOR('',#11032,1.);
#3264=VECTOR('',#11033,1.);
#3265=VECTOR('',#11036,1.);
#3266=VECTOR('',#11037,1.);
#3267=VECTOR('',#11038,1.);
#3268=VECTOR('',#11041,1.);
#3269=VECTOR('',#11042,1.);
#3270=VECTOR('',#11043,1.);
#3271=VECTOR('',#11046,1.);
#3272=VECTOR('',#11047,1.);
#3273=VECTOR('',#11058,0.425);
#3274=VECTOR('',#11065,0.645);
#3275=VECTOR('',#11078,0.425);
#3276=VECTOR('',#11085,0.645);
#3277=VECTOR('',#11098,0.34);
#3278=VECTOR('',#11107,0.34);
#3279=VECTOR('',#11116,0.5);
#3280=VECTOR('',#11127,0.5);
#3281=VECTOR('',#11138,0.5);
#3282=VECTOR('',#11149,0.5);
#3283=VECTOR('',#11160,0.275);
#3284=VECTOR('',#11165,0.275);
#3285=VECTOR('',#11170,0.275);
#3286=VECTOR('',#11175,0.275);
#3287=VECTOR('',#11178,1.);
#3288=VECTOR('',#11179,1.);
#3289=VECTOR('',#11180,1.);
#3290=VECTOR('',#11181,1.);
#3291=VECTOR('',#11184,1.);
#3292=VECTOR('',#11185,1.);
#3293=VECTOR('',#11186,1.);
#3294=VECTOR('',#11189,1.);
#3295=VECTOR('',#11190,1.);
#3296=VECTOR('',#11191,1.);
#3297=VECTOR('',#11194,1.);
#3298=VECTOR('',#11195,1.);
#3299=VECTOR('',#11206,0.425);
#3300=VECTOR('',#11213,0.645);
#3301=VECTOR('',#11226,0.425);
#3302=VECTOR('',#11233,0.645);
#3303=VECTOR('',#11244,0.4);
#3304=VECTOR('',#11247,1.);
#3305=VECTOR('',#11254,1.);
#3306=VECTOR('',#11257,1.);
#3307=VECTOR('',#11266,1.);
#3308=VECTOR('',#11275,1.);
#3309=VECTOR('',#11276,1.);
#3310=VECTOR('',#11277,1.);
#3311=VECTOR('',#11278,1.);
#3312=VECTOR('',#11279,1.);
#3313=VECTOR('',#11280,1.);
#3314=VECTOR('',#11293,0.225);
#3315=VECTOR('',#11298,0.225);
#3316=VECTOR('',#11303,0.21);
#3317=VECTOR('',#11310,0.21);
#3318=VECTOR('',#11317,0.21);
#3319=VECTOR('',#11324,0.21);
#3320=VECTOR('',#11329,1.);
#3321=VECTOR('',#11330,1.);
#3322=VECTOR('',#11331,1.);
#3323=VECTOR('',#11334,1.);
#3324=VECTOR('',#11335,1.);
#3325=VECTOR('',#11338,1.);
#3326=VECTOR('',#11339,1.);
#3327=VECTOR('',#11342,1.);
#3328=VECTOR('',#11349,0.399999999999999);
#3329=VECTOR('',#11352,1.);
#3330=VECTOR('',#11359,1.);
#3331=VECTOR('',#11362,1.);
#3332=VECTOR('',#11371,1.);
#3333=VECTOR('',#11380,1.);
#3334=VECTOR('',#11381,1.);
#3335=VECTOR('',#11382,1.);
#3336=VECTOR('',#11383,1.);
#3337=VECTOR('',#11384,1.);
#3338=VECTOR('',#11385,1.);
#3339=VECTOR('',#11398,0.225000000000001);
#3340=VECTOR('',#11403,0.225000000000001);
#3341=VECTOR('',#11408,0.210000000000001);
#3342=VECTOR('',#11415,0.210000000000001);
#3343=VECTOR('',#11422,0.210000000000001);
#3344=VECTOR('',#11429,0.210000000000001);
#3345=VECTOR('',#11434,1.);
#3346=VECTOR('',#11435,1.);
#3347=VECTOR('',#11436,1.);
#3348=VECTOR('',#11439,1.);
#3349=VECTOR('',#11440,1.);
#3350=VECTOR('',#11443,1.);
#3351=VECTOR('',#11444,1.);
#3352=VECTOR('',#11447,1.);
#3353=VECTOR('',#11454,1.);
#3354=VECTOR('',#11455,1.);
#3355=VECTOR('',#11456,1.);
#3356=VECTOR('',#11457,1.);
#3357=VECTOR('',#11460,1.);
#3358=VECTOR('',#11461,1.);
#3359=VECTOR('',#11462,1.);
#3360=VECTOR('',#11465,1.);
#3361=VECTOR('',#11466,1.);
#3362=VECTOR('',#11467,1.);
#3363=VECTOR('',#11470,1.);
#3364=VECTOR('',#11471,1.);
#3365=VECTOR('',#11480,1.);
#3366=VECTOR('',#11481,1.);
#3367=VECTOR('',#11482,1.);
#3368=VECTOR('',#11483,1.);
#3369=VECTOR('',#11486,1.);
#3370=VECTOR('',#11487,1.);
#3371=VECTOR('',#11488,1.);
#3372=VECTOR('',#11491,1.);
#3373=VECTOR('',#11492,1.);
#3374=VECTOR('',#11493,1.);
#3375=VECTOR('',#11496,1.);
#3376=VECTOR('',#11497,1.);
#3377=VECTOR('',#11512,0.4);
#3378=VECTOR('',#11517,0.425);
#3379=VECTOR('',#11522,0.41);
#3380=VECTOR('',#11531,0.26);
#3381=VECTOR('',#11536,0.25);
#3382=VECTOR('',#11541,0.225);
#3383=VECTOR('',#11546,1.);
#3384=VECTOR('',#11547,1.);
#3385=VECTOR('',#11548,1.);
#3386=VECTOR('',#11549,1.);
#3387=VECTOR('',#11552,1.);
#3388=VECTOR('',#11553,1.);
#3389=VECTOR('',#11554,1.);
#3390=VECTOR('',#11557,1.);
#3391=VECTOR('',#11558,1.);
#3392=VECTOR('',#11559,1.);
#3393=VECTOR('',#11562,1.);
#3394=VECTOR('',#11563,1.);
#3395=VECTOR('',#11564,1.);
#3396=VECTOR('',#11567,1.);
#3397=VECTOR('',#11568,1.);
#3398=VECTOR('',#11569,1.);
#3399=VECTOR('',#11572,1.);
#3400=VECTOR('',#11573,1.);
#3401=VECTOR('',#11586,2.05);
#3402=VECTOR('',#11593,2.05);
#3403=VECTOR('',#11602,1.);
#3404=VECTOR('',#11603,1.);
#3405=VECTOR('',#11608,1.);
#3406=VECTOR('',#11611,1.);
#3407=VECTOR('',#11614,1.);
#3408=VECTOR('',#11617,1.);
#3409=VECTOR('',#11620,1.);
#3410=VECTOR('',#11621,1.);
#3411=VECTOR('',#11624,1.);
#3412=VECTOR('',#11625,1.);
#3413=VECTOR('',#11630,1.);
#3414=VECTOR('',#11631,1.);
#3415=VECTOR('',#11634,1.);
#3416=VECTOR('',#11635,1.);
#3417=VECTOR('',#11636,1.);
#3418=VECTOR('',#11637,1.);
#3419=VECTOR('',#11642,1.);
#3420=VECTOR('',#11643,1.);
#3421=VECTOR('',#11644,1.);
#3422=VECTOR('',#11645,1.);
#3423=VECTOR('',#11646,1.);
#3424=VECTOR('',#11647,1.);
#3425=VECTOR('',#11660,1.);
#3426=VECTOR('',#11661,1.);
#3427=VECTOR('',#11662,1.);
#3428=VECTOR('',#11663,1.);
#3429=VECTOR('',#11666,1.);
#3430=VECTOR('',#11667,1.);
#3431=VECTOR('',#11668,1.);
#3432=VECTOR('',#11671,1.);
#3433=VECTOR('',#11672,1.);
#3434=VECTOR('',#11673,1.);
#3435=VECTOR('',#11676,1.);
#3436=VECTOR('',#11677,1.);
#3437=VECTOR('',#11684,0.65);
#3438=VECTOR('',#11689,0.65);
#3439=VECTOR('',#11692,1.);
#3440=VECTOR('',#11693,1.);
#3441=VECTOR('',#11694,1.);
#3442=VECTOR('',#11697,1.);
#3443=VECTOR('',#11698,1.);
#3444=VECTOR('',#11701,1.);
#3445=VECTOR('',#11702,1.);
#3446=VECTOR('',#11705,1.);
#3447=VECTOR('',#11714,1.8);
#3448=VECTOR('',#11731,0.25);
#3449=VECTOR('',#11734,0.25);
#3450=VECTOR('',#11739,1.65);
#3451=VECTOR('',#11744,0.25);
#3452=VECTOR('',#11747,0.25);
#3453=VECTOR('',#11750,0.25);
#3454=VECTOR('',#11753,0.25);
#3455=VECTOR('',#11766,1.75);
#3456=VECTOR('',#11773,1.);
#3457=VECTOR('',#11784,0.42);
#3458=VECTOR('',#11791,0.8);
#3459=VECTOR('',#11802,1.);
#3460=VECTOR('',#11803,1.);
#3461=VECTOR('',#11804,1.);
#3462=VECTOR('',#11805,1.);
#3463=VECTOR('',#11808,1.);
#3464=VECTOR('',#11809,1.);
#3465=VECTOR('',#11810,1.);
#3466=VECTOR('',#11813,1.);
#3467=VECTOR('',#11814,1.);
#3468=VECTOR('',#11815,1.);
#3469=VECTOR('',#11818,1.);
#3470=VECTOR('',#11819,1.);
#3471=VECTOR('',#11820,1.);
#3472=VECTOR('',#11823,1.);
#3473=VECTOR('',#11824,1.);
#3474=VECTOR('',#11825,1.);
#3475=VECTOR('',#11828,1.);
#3476=VECTOR('',#11829,1.);
#3477=VECTOR('',#11846,0.625);
#3478=VECTOR('',#11851,0.65);
#3479=VECTOR('',#11856,0.635);
#3480=VECTOR('',#11865,0.41);
#3481=VECTOR('',#11868,0.4);
#3482=VECTOR('',#11873,1.);
#3483=VECTOR('',#11878,1.);
#3484=VECTOR('',#11881,1.);
#3485=VECTOR('',#11884,1.);
#3486=VECTOR('',#11887,1.);
#3487=VECTOR('',#11892,1.);
#3488=VECTOR('',#11895,1.);
#3489=VECTOR('',#11896,1.);
#3490=VECTOR('',#11897,1.);
#3491=VECTOR('',#11898,1.);
#3492=VECTOR('',#11899,1.);
#3493=VECTOR('',#11904,1.);
#3494=VECTOR('',#11905,1.);
#3495=VECTOR('',#11906,1.);
#3496=VECTOR('',#11911,1.);
#3497=VECTOR('',#11912,1.);
#3498=VECTOR('',#11913,1.);
#3499=VECTOR('',#11914,1.);
#3500=VECTOR('',#11915,1.);
#3501=VECTOR('',#11922,0.225);
#3502=VECTOR('',#11927,0.165);
#3503=VECTOR('',#11934,0.275);
#3504=VECTOR('',#11939,0.275);
#3505=VECTOR('',#11944,0.6);
#3506=VECTOR('',#11949,1.);
#3507=VECTOR('',#11950,1.);
#3508=VECTOR('',#11951,1.);
#3509=VECTOR('',#11952,1.);
#3510=VECTOR('',#11953,1.);
#3511=VECTOR('',#11954,1.);
#3512=VECTOR('',#11955,1.);
#3513=VECTOR('',#11956,1.);
#3514=VECTOR('',#11957,1.);
#3515=VECTOR('',#11960,1.);
#3516=VECTOR('',#11961,1.);
#3517=VECTOR('',#11964,1.);
#3518=VECTOR('',#11965,1.);
#3519=VECTOR('',#11968,1.);
#3520=VECTOR('',#11971,1.);
#3521=VECTOR('',#11972,1.);
#3522=VECTOR('',#11975,1.);
#3523=VECTOR('',#11976,1.);
#3524=VECTOR('',#11979,1.);
#3525=VECTOR('',#11980,1.);
#3526=VECTOR('',#11983,1.);
#3527=VECTOR('',#11984,1.);
#3528=VECTOR('',#11987,1.);
#3529=VECTOR('',#11988,1.);
#3530=VECTOR('',#11991,1.);
#3531=VECTOR('',#12000,0.275);
#3532=VECTOR('',#12005,0.265);
#3533=VECTOR('',#12014,0.5);
#3534=VECTOR('',#12023,1.);
#3535=VECTOR('',#12024,1.);
#3536=VECTOR('',#12025,1.);
#3537=VECTOR('',#12026,1.);
#3538=VECTOR('',#12029,1.);
#3539=VECTOR('',#12030,1.);
#3540=VECTOR('',#12031,1.);
#3541=VECTOR('',#12034,1.);
#3542=VECTOR('',#12035,1.);
#3543=VECTOR('',#12036,1.);
#3544=VECTOR('',#12039,1.);
#3545=VECTOR('',#12040,1.);
#3546=VECTOR('',#12041,1.);
#3547=VECTOR('',#12044,1.);
#3548=VECTOR('',#12045,1.);
#3549=VECTOR('',#12046,1.);
#3550=VECTOR('',#12049,1.);
#3551=VECTOR('',#12050,1.);
#3552=VECTOR('',#12067,0.4);
#3553=VECTOR('',#12072,0.425);
#3554=VECTOR('',#12077,0.41);
#3555=VECTOR('',#12086,0.26);
#3556=VECTOR('',#12089,0.25);
#3557=VECTOR('',#12100,0.325);
#3558=VECTOR('',#12105,0.35);
#3559=VECTOR('',#12110,0.335);
#3560=VECTOR('',#12119,0.21);
#3561=VECTOR('',#12124,0.2);
#3562=VECTOR('',#12129,0.18);
#3563=VECTOR('',#12134,1.);
#3564=VECTOR('',#12135,1.);
#3565=VECTOR('',#12136,1.);
#3566=VECTOR('',#12137,1.);
#3567=VECTOR('',#12140,1.);
#3568=VECTOR('',#12141,1.);
#3569=VECTOR('',#12142,1.);
#3570=VECTOR('',#12145,1.);
#3571=VECTOR('',#12146,1.);
#3572=VECTOR('',#12147,1.);
#3573=VECTOR('',#12150,1.);
#3574=VECTOR('',#12151,1.);
#3575=VECTOR('',#12152,1.);
#3576=VECTOR('',#12155,1.);
#3577=VECTOR('',#12156,1.);
#3578=VECTOR('',#12157,1.);
#3579=VECTOR('',#12160,1.);
#3580=VECTOR('',#12161,1.);
#3581=VECTOR('',#12176,0.55);
#3582=VECTOR('',#12181,0.6);
#3583=VECTOR('',#12190,1.);
#3584=VECTOR('',#12191,1.);
#3585=VECTOR('',#12192,1.);
#3586=VECTOR('',#12193,1.);
#3587=VECTOR('',#12198,1.);
#3588=VECTOR('',#12199,1.);
#3589=VECTOR('',#12202,1.);
#3590=VECTOR('',#12203,1.);
#3591=VECTOR('',#12204,1.);
#3592=VECTOR('',#12207,1.);
#3593=VECTOR('',#12212,1.);
#3594=VECTOR('',#12225,1.);
#3595=VECTOR('',#12232,0.21);
#3596=VECTOR('',#12237,1.);
#3597=VECTOR('',#12242,1.005);
#3598=VECTOR('',#12249,1.5);
#3599=VECTOR('',#12260,1.);
#3600=VECTOR('',#12267,0.21);
#3601=VECTOR('',#12272,1.);
#3602=VECTOR('',#12277,1.005);
#3603=VECTOR('',#12284,1.5);
#3604=VECTOR('',#12297,1.005);
#3605=VECTOR('',#12304,1.3);
#3606=VECTOR('',#12315,1.);
#3607=VECTOR('',#12318,1.);
#3608=VECTOR('',#12325,1.);
#3609=VECTOR('',#12326,1.);
#3610=VECTOR('',#12327,1.);
#3611=VECTOR('',#12334,0.34);
#3612=VECTOR('',#12341,1.);
#3613=VECTOR('',#12348,1.);
#3614=VECTOR('',#12349,1.);
#3615=VECTOR('',#12352,1.);
#3616=VECTOR('',#12357,1.);
#3617=VECTOR('',#12358,1.);
#3618=VECTOR('',#12363,1.);
#3619=VECTOR('',#12364,1.);
#3620=VECTOR('',#12367,1.);
#3621=VECTOR('',#12368,1.);
#3622=VECTOR('',#12371,1.);
#3623=VECTOR('',#12386,4.);
#3624=VECTOR('',#12389,1.6);
#3625=VECTOR('',#12404,0.165);
#3626=VECTOR('',#12419,0.5);
#3627=VECTOR('',#12424,0.4);
#3628=VECTOR('',#12435,0.505);
#3629=VECTOR('',#12442,0.7);
#3630=VECTOR('',#12455,0.505);
#3631=VECTOR('',#12462,0.7);
#3632=VECTOR('',#12475,0.225);
#3633=VECTOR('',#12482,0.8);
#3634=VECTOR('',#12493,1.);
#3635=VECTOR('',#12494,1.);
#3636=VECTOR('',#12495,1.);
#3637=VECTOR('',#12496,1.);
#3638=VECTOR('',#12497,1.);
#3639=VECTOR('',#12498,1.);
#3640=VECTOR('',#12499,1.);
#3641=VECTOR('',#12500,1.);
#3642=VECTOR('',#12503,1.);
#3643=VECTOR('',#12504,1.);
#3644=VECTOR('',#12505,1.);
#3645=VECTOR('',#12508,1.);
#3646=VECTOR('',#12509,1.);
#3647=VECTOR('',#12512,1.);
#3648=VECTOR('',#12513,1.);
#3649=VECTOR('',#12516,1.);
#3650=VECTOR('',#12517,1.);
#3651=VECTOR('',#12520,1.);
#3652=VECTOR('',#12521,1.);
#3653=VECTOR('',#12522,1.);
#3654=VECTOR('',#12523,1.);
#3655=VECTOR('',#12526,1.);
#3656=VECTOR('',#12529,1.);
#3657=VECTOR('',#12532,1.);
#3658=VECTOR('',#12539,1.);
#3659=VECTOR('',#12540,1.);
#3660=VECTOR('',#12541,1.);
#3661=VECTOR('',#12542,1.);
#3662=VECTOR('',#12545,1.);
#3663=VECTOR('',#12546,1.);
#3664=VECTOR('',#12547,1.);
#3665=VECTOR('',#12550,1.);
#3666=VECTOR('',#12551,1.);
#3667=VECTOR('',#12552,1.);
#3668=VECTOR('',#12555,1.);
#3669=VECTOR('',#12556,1.);
#3670=VECTOR('',#12557,1.);
#3671=VECTOR('',#12560,1.);
#3672=VECTOR('',#12561,1.);
#3673=VECTOR('',#12562,1.);
#3674=VECTOR('',#12565,1.);
#3675=VECTOR('',#12566,1.);
#3676=VECTOR('',#12577,0.235);
#3677=VECTOR('',#12582,0.25);
#3678=VECTOR('',#12587,0.2125);
#3679=VECTOR('',#12598,1.5);
#3680=VECTOR('',#12605,1.5);
#3681=VECTOR('',#12610,1.);
#3682=VECTOR('',#12613,1.);
#3683=VECTOR('',#12618,1.);
#3684=VECTOR('',#12621,1.);
#3685=VECTOR('',#12624,1.);
#3686=VECTOR('',#12625,1.);
#3687=VECTOR('',#12628,1.);
#3688=VECTOR('',#12633,1.);
#3689=VECTOR('',#12642,1.1);
#3690=VECTOR('',#12649,2.);
#3691=VECTOR('',#12662,1.1);
#3692=VECTOR('',#12669,2.);
#3693=VECTOR('',#12682,1.1);
#3694=VECTOR('',#12689,2.);
#3695=VECTOR('',#12702,1.1);
#3696=VECTOR('',#12709,2.);
#3697=VECTOR('',#12734,0.976185);
#3698=VECTOR('',#12741,0.5);
#3699=VECTOR('',#12746,0.53);
#3700=VECTOR('',#12755,0.976185);
#3701=VECTOR('',#12762,0.53);
#3702=VECTOR('',#12781,1.023815);
#3703=VECTOR('',#12792,1.47);
#3704=VECTOR('',#12797,1.5);
#3705=VECTOR('',#12802,1.47);
#3706=VECTOR('',#12807,1.023815);
#3707=VECTOR('',#12858,1.019052);
#3708=VECTOR('',#12935,0.980948);
#3709=VECTOR('',#12964,1.013815);
#3710=VECTOR('',#12971,0.991185);
#3711=VECTOR('',#12982,1.013815);
#3712=VECTOR('',#12989,0.991185);
#3713=VECTOR('',#13022,0.5);
#3714=VECTOR('',#13027,1.);
#3715=VECTOR('',#13028,1.);
#3716=VECTOR('',#13029,1.);
#3717=VECTOR('',#13030,1.);
#3718=VECTOR('',#13033,1.);
#3719=VECTOR('',#13034,1.);
#3720=VECTOR('',#13035,1.);
#3721=VECTOR('',#13038,1.);
#3722=VECTOR('',#13039,1.);
#3723=VECTOR('',#13040,1.);
#3724=VECTOR('',#13043,1.);
#3725=VECTOR('',#13046,1.);
#3726=VECTOR('',#13051,0.165);
#3727=VECTOR('',#13058,0.165);
#3728=VECTOR('',#13065,0.165);
#3729=VECTOR('',#13072,0.165);
#3730=VECTOR('',#13079,1.05);
#3731=VECTOR('',#13086,1.05);
#3732=VECTOR('',#13091,1.);
#3733=VECTOR('',#13092,1.);
#3734=VECTOR('',#13093,1.);
#3735=VECTOR('',#13094,1.);
#3736=VECTOR('',#13097,1.);
#3737=VECTOR('',#13098,1.);
#3738=VECTOR('',#13099,1.);
#3739=VECTOR('',#13102,1.);
#3740=VECTOR('',#13103,1.);
#3741=VECTOR('',#13104,1.);
#3742=VECTOR('',#13107,1.);
#3743=VECTOR('',#13108,1.);
#3744=VECTOR('',#13119,0.225);
#3745=VECTOR('',#13126,0.225);
#3746=VECTOR('',#13133,0.225);
#3747=VECTOR('',#13140,0.225);
#3748=VECTOR('',#13147,0.7);
#3749=VECTOR('',#13154,0.7);
#3750=VECTOR('',#13159,1.);
#3751=VECTOR('',#13160,1.);
#3752=VECTOR('',#13161,1.);
#3753=VECTOR('',#13162,1.);
#3754=VECTOR('',#13165,1.);
#3755=VECTOR('',#13166,1.);
#3756=VECTOR('',#13167,1.);
#3757=VECTOR('',#13170,1.);
#3758=VECTOR('',#13171,1.);
#3759=VECTOR('',#13172,1.);
#3760=VECTOR('',#13175,1.);
#3761=VECTOR('',#13176,1.);
#3762=VECTOR('',#13187,0.225);
#3763=VECTOR('',#13194,0.225);
#3764=VECTOR('',#13201,0.225);
#3765=VECTOR('',#13208,0.225);
#3766=VECTOR('',#13215,0.7);
#3767=VECTOR('',#13222,0.7);
#3768=VECTOR('',#13227,1.);
#3769=VECTOR('',#13228,1.);
#3770=VECTOR('',#13229,1.);
#3771=VECTOR('',#13230,1.);
#3772=VECTOR('',#13233,1.);
#3773=VECTOR('',#13234,1.);
#3774=VECTOR('',#13235,1.);
#3775=VECTOR('',#13238,1.);
#3776=VECTOR('',#13239,1.);
#3777=VECTOR('',#13240,1.);
#3778=VECTOR('',#13243,1.);
#3779=VECTOR('',#13244,1.);
#3780=VECTOR('',#13255,0.164999999999999);
#3781=VECTOR('',#13268,0.800000000000001);
#3782=VECTOR('',#13277,0.5);
#3783=VECTOR('',#13286,0.505000000000001);
#3784=VECTOR('',#13293,0.699999999999999);
#3785=VECTOR('',#13306,0.505000000000001);
#3786=VECTOR('',#13313,0.699999999999999);
#3787=VECTOR('',#13326,0.225);
#3788=VECTOR('',#13333,0.800000000000001);
#3789=VECTOR('',#13348,1.);
#3790=VECTOR('',#13349,1.);
#3791=VECTOR('',#13350,1.);
#3792=VECTOR('',#13353,1.);
#3793=VECTOR('',#13354,1.);
#3794=VECTOR('',#13355,1.);
#3795=VECTOR('',#13360,1.);
#3796=VECTOR('',#13361,1.);
#3797=VECTOR('',#13364,1.);
#3798=VECTOR('',#13365,1.);
#3799=VECTOR('',#13378,1.05);
#3800=VECTOR('',#13387,1.);
#3801=VECTOR('',#13396,1.05);
#3802=VECTOR('',#13405,1.);
#3803=VECTOR('',#13414,1.05);
#3804=VECTOR('',#13421,0.9);
#3805=VECTOR('',#13428,1.);
#3806=VECTOR('',#13431,1.);
#3807=VECTOR('',#13434,1.);
#3808=VECTOR('',#13435,1.);
#3809=VECTOR('',#13436,1.);
#3810=VECTOR('',#13443,1.);
#3811=VECTOR('',#13446,1.);
#3812=VECTOR('',#13447,1.);
#3813=VECTOR('',#13458,0.895);
#3814=VECTOR('',#13465,0.605);
#3815=VECTOR('',#13474,1.);
#3816=VECTOR('',#13475,1.);
#3817=VECTOR('',#13476,1.);
#3818=VECTOR('',#13477,1.);
#3819=VECTOR('',#13480,1.);
#3820=VECTOR('',#13481,1.);
#3821=VECTOR('',#13482,1.);
#3822=VECTOR('',#13485,1.);
#3823=VECTOR('',#13486,1.);
#3824=VECTOR('',#13487,1.);
#3825=VECTOR('',#13490,1.);
#3826=VECTOR('',#13491,1.);
#3827=VECTOR('',#13492,1.);
#3828=VECTOR('',#13495,1.);
#3829=VECTOR('',#13496,1.);
#3830=VECTOR('',#13497,1.);
#3831=VECTOR('',#13500,1.);
#3832=VECTOR('',#13501,1.);
#3833=VECTOR('',#13518,0.325);
#3834=VECTOR('',#13523,0.35);
#3835=VECTOR('',#13528,0.335);
#3836=VECTOR('',#13537,0.21);
#3837=VECTOR('',#13540,0.2);
#3838=CIRCLE('',#9689,0.164999999999999);
#3839=CIRCLE('',#9690,0.164999999999999);
#3840=CIRCLE('',#9692,0.164999999999999);
#3841=CIRCLE('',#9693,0.164999999999999);
#3842=CIRCLE('',#9695,0.165);
#3843=CIRCLE('',#9696,0.165);
#3844=CIRCLE('',#9698,0.165);
#3845=CIRCLE('',#9699,0.165);
#3846=CIRCLE('',#9701,0.21);
#3847=CIRCLE('',#9702,0.21);
#3848=CIRCLE('',#9704,0.21);
#3849=CIRCLE('',#9705,0.21);
#3850=CIRCLE('',#9707,0.21);
#3851=CIRCLE('',#9708,0.21);
#3852=CIRCLE('',#9710,0.21);
#3853=CIRCLE('',#9711,0.21);
#3854=CIRCLE('',#9713,0.21);
#3855=CIRCLE('',#9714,0.21);
#3856=CIRCLE('',#9716,0.21);
#3857=CIRCLE('',#9717,0.21);
#3858=CIRCLE('',#9719,0.21);
#3859=CIRCLE('',#9720,0.21);
#3860=CIRCLE('',#9722,0.21);
#3861=CIRCLE('',#9723,0.21);
#3862=CIRCLE('',#9732,0.34);
#3863=CIRCLE('',#9733,0.34);
#3864=CIRCLE('',#9736,0.34);
#3865=CIRCLE('',#9737,0.34);
#3866=CIRCLE('',#9740,0.5);
#3867=CIRCLE('',#9741,0.5);
#3868=CIRCLE('',#9743,0.275);
#3869=CIRCLE('',#9745,0.5);
#3870=CIRCLE('',#9746,0.5);
#3871=CIRCLE('',#9748,0.275);
#3872=CIRCLE('',#9750,0.5);
#3873=CIRCLE('',#9751,0.5);
#3874=CIRCLE('',#9753,0.275);
#3875=CIRCLE('',#9755,0.5);
#3876=CIRCLE('',#9756,0.5);
#3877=CIRCLE('',#9758,0.275);
#3878=CIRCLE('',#9760,0.275);
#3879=CIRCLE('',#9762,0.275);
#3880=CIRCLE('',#9764,0.275);
#3881=CIRCLE('',#9766,0.275);
#3882=CIRCLE('',#9775,0.425);
#3883=CIRCLE('',#9776,0.425);
#3884=CIRCLE('',#9778,0.645);
#3885=CIRCLE('',#9779,0.645);
#3886=CIRCLE('',#9784,0.425);
#3887=CIRCLE('',#9785,0.425);
#3888=CIRCLE('',#9787,0.645);
#3889=CIRCLE('',#9788,0.645);
#3890=CIRCLE('',#9793,0.34);
#3891=CIRCLE('',#9794,0.34);
#3892=CIRCLE('',#9797,0.34);
#3893=CIRCLE('',#9798,0.34);
#3894=CIRCLE('',#9801,0.5);
#3895=CIRCLE('',#9802,0.5);
#3896=CIRCLE('',#9804,0.275);
#3897=CIRCLE('',#9806,0.5);
#3898=CIRCLE('',#9807,0.5);
#3899=CIRCLE('',#9809,0.275);
#3900=CIRCLE('',#9811,0.5);
#3901=CIRCLE('',#9812,0.5);
#3902=CIRCLE('',#9814,0.275);
#3903=CIRCLE('',#9816,0.5);
#3904=CIRCLE('',#9817,0.5);
#3905=CIRCLE('',#9819,0.275);
#3906=CIRCLE('',#9821,0.275);
#3907=CIRCLE('',#9823,0.275);
#3908=CIRCLE('',#9825,0.275);
#3909=CIRCLE('',#9827,0.275);
#3910=CIRCLE('',#9836,0.425);
#3911=CIRCLE('',#9837,0.425);
#3912=CIRCLE('',#9839,0.645);
#3913=CIRCLE('',#9840,0.645);
#3914=CIRCLE('',#9845,0.425);
#3915=CIRCLE('',#9846,0.425);
#3916=CIRCLE('',#9848,0.645);
#3917=CIRCLE('',#9849,0.645);
#3918=CIRCLE('',#9854,0.4);
#3919=CIRCLE('',#9855,0.4);
#3920=CIRCLE('',#9857,0.4);
#3921=CIRCLE('',#9858,0.4);
#3922=CIRCLE('',#9860,0.225);
#3923=CIRCLE('',#9862,0.4);
#3924=CIRCLE('',#9863,0.4);
#3925=CIRCLE('',#9865,0.225);
#3926=CIRCLE('',#9867,0.21);
#3927=CIRCLE('',#9868,0.21);
#3928=CIRCLE('',#9869,0.21);
#3929=CIRCLE('',#9870,0.21);
#3930=CIRCLE('',#9872,0.225);
#3931=CIRCLE('',#9874,0.225);
#3932=CIRCLE('',#9876,0.21);
#3933=CIRCLE('',#9879,0.21);
#3934=CIRCLE('',#9882,0.21);
#3935=CIRCLE('',#9885,0.21);
#3936=CIRCLE('',#9894,0.399999999999999);
#3937=CIRCLE('',#9895,0.399999999999999);
#3938=CIRCLE('',#9897,0.399999999999999);
#3939=CIRCLE('',#9898,0.399999999999999);
#3940=CIRCLE('',#9900,0.225000000000001);
#3941=CIRCLE('',#9902,0.399999999999999);
#3942=CIRCLE('',#9903,0.399999999999999);
#3943=CIRCLE('',#9905,0.225000000000001);
#3944=CIRCLE('',#9907,0.210000000000001);
#3945=CIRCLE('',#9908,0.210000000000001);
#3946=CIRCLE('',#9909,0.210000000000001);
#3947=CIRCLE('',#9910,0.210000000000001);
#3948=CIRCLE('',#9912,0.225000000000001);
#3949=CIRCLE('',#9914,0.225000000000001);
#3950=CIRCLE('',#9916,0.210000000000001);
#3951=CIRCLE('',#9919,0.210000000000001);
#3952=CIRCLE('',#9922,0.210000000000001);
#3953=CIRCLE('',#9925,0.210000000000001);
#3954=CIRCLE('',#9948,0.375);
#3955=CIRCLE('',#9950,0.425);
#3956=CIRCLE('',#9952,0.425);
#3957=CIRCLE('',#9954,0.395);
#3958=CIRCLE('',#9956,0.27);
#3959=CIRCLE('',#9958,0.24505);
#3960=CIRCLE('',#9960,0.24505);
#3961=CIRCLE('',#9962,0.2);
#3962=CIRCLE('',#9975,2.05);
#3963=CIRCLE('',#9976,2.05);
#3964=CIRCLE('',#9978,2.05);
#3965=CIRCLE('',#9979,2.05);
#3966=CIRCLE('',#9981,2.35);
#3967=CIRCLE('',#9983,2.8);
#3968=CIRCLE('',#9985,2.8);
#3969=CIRCLE('',#9987,2.8);
#3970=CIRCLE('',#9990,2.8);
#3971=CIRCLE('',#9993,0.65);
#3972=CIRCLE('',#9994,0.65);
#3973=CIRCLE('',#9996,2.8);
#3974=CIRCLE('',#9997,2.8);
#3975=CIRCLE('',#10006,0.65);
#3976=CIRCLE('',#10008,0.65);
#3977=CIRCLE('',#10016,1.8);
#3978=CIRCLE('',#10017,1.8);
#3979=CIRCLE('',#10019,2.19089023002066);
#3980=CIRCLE('',#10021,2.35);
#3981=CIRCLE('',#10022,2.19089023002066);
#3982=CIRCLE('',#10027,1.65);
#3983=CIRCLE('',#10028,1.65);
#3984=CIRCLE('',#10034,1.);
#3985=CIRCLE('',#10036,1.75);
#3986=CIRCLE('',#10038,1.75);
#3987=CIRCLE('',#10040,1.);
#3988=CIRCLE('',#10046,0.42);
#3989=CIRCLE('',#10047,0.42);
#3990=CIRCLE('',#10049,0.8);
#3991=CIRCLE('',#10050,0.8);
#3992=CIRCLE('',#10063,0.3933);
#3993=CIRCLE('',#10065,0.6);
#3994=CIRCLE('',#10067,0.65);
#3995=CIRCLE('',#10069,0.65);
#3996=CIRCLE('',#10071,0.62);
#3997=CIRCLE('',#10073,0.42);
#3998=CIRCLE('',#10075,0.3933);
#3999=CIRCLE('',#10079,0.525);
#4000=CIRCLE('',#10081,0.525);
#4001=CIRCLE('',#10083,0.525);
#4002=CIRCLE('',#10084,0.525);
#4003=CIRCLE('',#10087,0.275);
#4004=CIRCLE('',#10089,0.165);
#4005=CIRCLE('',#10091,0.275);
#4006=CIRCLE('',#10093,0.225);
#4007=CIRCLE('',#10094,0.225);
#4008=CIRCLE('',#10096,0.165);
#4009=CIRCLE('',#10098,0.275);
#4010=CIRCLE('',#10100,0.275);
#4011=CIRCLE('',#10102,0.6);
#4012=CIRCLE('',#10103,0.6);
#4013=CIRCLE('',#10117,0.285);
#4014=CIRCLE('',#10118,0.265);
#4015=CIRCLE('',#10120,0.265);
#4016=CIRCLE('',#10122,0.5);
#4017=CIRCLE('',#10124,0.5);
#4018=CIRCLE('',#10136,0.24505);
#4019=CIRCLE('',#10138,0.375);
#4020=CIRCLE('',#10140,0.425);
#4021=CIRCLE('',#10142,0.425);
#4022=CIRCLE('',#10144,0.395);
#4023=CIRCLE('',#10146,0.27);
#4024=CIRCLE('',#10148,0.24505);
#4025=CIRCLE('',#10152,0.3);
#4026=CIRCLE('',#10154,0.35);
#4027=CIRCLE('',#10156,0.35);
#4028=CIRCLE('',#10158,0.32);
#4029=CIRCLE('',#10160,0.22);
#4030=CIRCLE('',#10162,0.1954);
#4031=CIRCLE('',#10164,0.1954);
#4032=CIRCLE('',#10166,0.16);
#4033=CIRCLE('',#10178,0.6);
#4034=CIRCLE('',#10180,0.6);
#4035=CIRCLE('',#10181,0.5);
#4036=CIRCLE('',#10188,1.);
#4037=CIRCLE('',#10192,1.);
#4038=CIRCLE('',#10193,1.);
#4039=CIRCLE('',#10194,1.);
#4040=CIRCLE('',#10199,0.21);
#4041=CIRCLE('',#10201,0.21);
#4042=CIRCLE('',#10202,0.21);
#4043=CIRCLE('',#10205,1.005);
#4044=CIRCLE('',#10206,1.005);
#4045=CIRCLE('',#10208,1.5);
#4046=CIRCLE('',#10209,1.5);
#4047=CIRCLE('',#10214,0.21);
#4048=CIRCLE('',#10216,0.21);
#4049=CIRCLE('',#10217,0.21);
#4050=CIRCLE('',#10220,1.005);
#4051=CIRCLE('',#10221,1.005);
#4052=CIRCLE('',#10223,1.5);
#4053=CIRCLE('',#10224,1.5);
#4054=CIRCLE('',#10229,1.005);
#4055=CIRCLE('',#10230,1.005);
#4056=CIRCLE('',#10232,1.3);
#4057=CIRCLE('',#10233,1.3);
#4058=CIRCLE('',#10238,0.5);
#4059=CIRCLE('',#10239,0.5);
#4060=CIRCLE('',#10241,1.6);
#4061=CIRCLE('',#10242,1.);
#4062=CIRCLE('',#10244,0.34);
#4063=CIRCLE('',#10245,0.34);
#4064=CIRCLE('',#10248,0.21);
#4065=CIRCLE('',#10250,0.21);
#4066=CIRCLE('',#10253,1.);
#4067=CIRCLE('',#10254,1.);
#4068=CIRCLE('',#10259,4.);
#4069=CIRCLE('',#10260,1.6);
#4070=CIRCLE('',#10262,4.);
#4071=CIRCLE('',#10263,1.6);
#4072=CIRCLE('',#10266,1.6);
#4073=CIRCLE('',#10267,1.6);
#4074=CIRCLE('',#10272,0.165);
#4075=CIRCLE('',#10273,0.165);
#4076=CIRCLE('',#10276,0.5);
#4077=CIRCLE('',#10277,0.4);
#4078=CIRCLE('',#10279,0.5);
#4079=CIRCLE('',#10282,0.4);
#4080=CIRCLE('',#10286,0.505);
#4081=CIRCLE('',#10287,0.505);
#4082=CIRCLE('',#10289,0.7);
#4083=CIRCLE('',#10290,0.7);
#4084=CIRCLE('',#10295,0.505);
#4085=CIRCLE('',#10296,0.505);
#4086=CIRCLE('',#10298,0.7);
#4087=CIRCLE('',#10299,0.7);
#4088=CIRCLE('',#10304,0.225);
#4089=CIRCLE('',#10305,0.225);
#4090=CIRCLE('',#10307,0.8);
#4091=CIRCLE('',#10308,0.8);
#4092=CIRCLE('',#10331,0.22);
#4093=CIRCLE('',#10333,0.24505);
#4094=CIRCLE('',#10335,0.24505);
#4095=CIRCLE('',#10337,0.175);
#4096=CIRCLE('',#10342,1.5);
#4097=CIRCLE('',#10343,1.5);
#4098=CIRCLE('',#10345,1.5);
#4099=CIRCLE('',#10346,1.5);
#4100=CIRCLE('',#10348,2.);
#4101=CIRCLE('',#10349,2.);
#4102=CIRCLE('',#10351,2.);
#4103=CIRCLE('',#10354,2.);
#4104=CIRCLE('',#10359,1.1);
#4105=CIRCLE('',#10360,1.1);
#4106=CIRCLE('',#10362,2.);
#4107=CIRCLE('',#10363,2.);
#4108=CIRCLE('',#10368,1.1);
#4109=CIRCLE('',#10369,1.1);
#4110=CIRCLE('',#10371,2.);
#4111=CIRCLE('',#10372,2.);
#4112=CIRCLE('',#10377,1.1);
#4113=CIRCLE('',#10378,1.1);
#4114=CIRCLE('',#10380,2.);
#4115=CIRCLE('',#10381,2.);
#4116=CIRCLE('',#10386,1.1);
#4117=CIRCLE('',#10387,1.1);
#4118=CIRCLE('',#10389,2.);
#4119=CIRCLE('',#10390,2.);
#4120=CIRCLE('',#10396,0.976185);
#4121=CIRCLE('',#10397,0.976185);
#4122=CIRCLE('',#10398,0.247676);
#4123=CIRCLE('',#10399,0.976185);
#4124=CIRCLE('',#10400,0.976185);
#4125=CIRCLE('',#10402,0.976185);
#4126=CIRCLE('',#10404,0.5);
#4127=CIRCLE('',#10405,0.5);
#4128=CIRCLE('',#10407,0.56);
#4129=CIRCLE('',#10410,0.976185);
#4130=CIRCLE('',#10412,0.56);
#4131=CIRCLE('',#10416,1.023815);
#4132=CIRCLE('',#10417,1.023815);
#4133=CIRCLE('',#10418,0.247676);
#4134=CIRCLE('',#10419,1.023815);
#4135=CIRCLE('',#10420,1.023815);
#4136=CIRCLE('',#10422,1.023815);
#4137=CIRCLE('',#10424,1.44);
#4138=CIRCLE('',#10425,1.023815);
#4139=CIRCLE('',#10427,1.5);
#4140=CIRCLE('',#10429,1.5);
#4141=CIRCLE('',#10431,1.44);
#4142=CIRCLE('',#10436,0.23815);
#4143=CIRCLE('',#10438,0.23815);
#4144=CIRCLE('',#10440,0.23815);
#4145=CIRCLE('',#10442,0.23815);
#4146=CIRCLE('',#10444,0.23815);
#4147=CIRCLE('',#10446,0.23815);
#4148=CIRCLE('',#10448,0.23815);
#4149=CIRCLE('',#10450,0.23815);
#4150=CIRCLE('',#10453,0.243053047864041);
#4151=CIRCLE('',#10454,0.243053047864041);
#4152=CIRCLE('',#10456,1.019052);
#4153=CIRCLE('',#10457,1.019052);
#4154=CIRCLE('',#10458,1.019052);
#4155=CIRCLE('',#10459,1.019052);
#4156=CIRCLE('',#10460,1.019052);
#4157=CIRCLE('',#10461,1.019052);
#4158=CIRCLE('',#10462,1.019052);
#4159=CIRCLE('',#10463,1.019052);
#4160=CIRCLE('',#10464,1.019052);
#4161=CIRCLE('',#10466,0.980948);
#4162=CIRCLE('',#10467,0.243053047864041);
#4163=CIRCLE('',#10469,0.243053047864041);
#4164=CIRCLE('',#10471,0.980948);
#4165=CIRCLE('',#10472,0.243053047864041);
#4166=CIRCLE('',#10474,0.243053047864041);
#4167=CIRCLE('',#10476,0.980948);
#4168=CIRCLE('',#10477,0.243053047864041);
#4169=CIRCLE('',#10479,0.243053047864041);
#4170=CIRCLE('',#10481,0.980948);
#4171=CIRCLE('',#10482,0.243053047864041);
#4172=CIRCLE('',#10484,0.243053047864041);
#4173=CIRCLE('',#10486,0.980948);
#4174=CIRCLE('',#10487,0.243053047864041);
#4175=CIRCLE('',#10489,0.243053047864041);
#4176=CIRCLE('',#10491,0.980948);
#4177=CIRCLE('',#10492,0.243053047864041);
#4178=CIRCLE('',#10494,0.243053047864041);
#4179=CIRCLE('',#10496,0.980948);
#4180=CIRCLE('',#10497,0.980948);
#4181=CIRCLE('',#10498,0.980948);
#4182=CIRCLE('',#10500,0.243053047864041);
#4183=CIRCLE('',#10502,0.243053047864041);
#4184=CIRCLE('',#10507,1.013815);
#4185=CIRCLE('',#10508,0.991185);
#4186=CIRCLE('',#10510,1.013815);
#4187=CIRCLE('',#10512,0.991185);
#4188=CIRCLE('',#10515,1.013815);
#4189=CIRCLE('',#10516,0.991185);
#4190=CIRCLE('',#10518,1.013815);
#4191=CIRCLE('',#10520,0.991185);
#4192=CIRCLE('',#10537,0.5);
#4193=CIRCLE('',#10538,0.5);
#4194=CIRCLE('',#10545,0.165);
#4195=CIRCLE('',#10546,0.165);
#4196=CIRCLE('',#10548,0.165);
#4197=CIRCLE('',#10549,0.165);
#4198=CIRCLE('',#10551,0.165);
#4199=CIRCLE('',#10552,0.165);
#4200=CIRCLE('',#10554,0.165);
#4201=CIRCLE('',#10555,0.165);
#4202=CIRCLE('',#10557,1.05);
#4203=CIRCLE('',#10558,1.05);
#4204=CIRCLE('',#10560,1.05);
#4205=CIRCLE('',#10561,1.05);
#4206=CIRCLE('',#10570,0.225);
#4207=CIRCLE('',#10571,0.225);
#4208=CIRCLE('',#10573,0.225);
#4209=CIRCLE('',#10574,0.225);
#4210=CIRCLE('',#10576,0.225);
#4211=CIRCLE('',#10577,0.225);
#4212=CIRCLE('',#10579,0.225);
#4213=CIRCLE('',#10580,0.225);
#4214=CIRCLE('',#10582,0.7);
#4215=CIRCLE('',#10583,0.7);
#4216=CIRCLE('',#10585,0.7);
#4217=CIRCLE('',#10586,0.7);
#4218=CIRCLE('',#10595,0.225);
#4219=CIRCLE('',#10596,0.225);
#4220=CIRCLE('',#10598,0.225);
#4221=CIRCLE('',#10599,0.225);
#4222=CIRCLE('',#10601,0.225);
#4223=CIRCLE('',#10602,0.225);
#4224=CIRCLE('',#10604,0.225);
#4225=CIRCLE('',#10605,0.225);
#4226=CIRCLE('',#10607,0.7);
#4227=CIRCLE('',#10608,0.7);
#4228=CIRCLE('',#10610,0.7);
#4229=CIRCLE('',#10611,0.7);
#4230=CIRCLE('',#10620,0.164999999999999);
#4231=CIRCLE('',#10621,0.164999999999999);
#4232=CIRCLE('',#10624,0.800000000000001);
#4233=CIRCLE('',#10625,0.5);
#4234=CIRCLE('',#10627,0.800000000000001);
#4235=CIRCLE('',#10630,0.5);
#4236=CIRCLE('',#10634,0.505000000000001);
#4237=CIRCLE('',#10635,0.505000000000001);
#4238=CIRCLE('',#10637,0.699999999999999);
#4239=CIRCLE('',#10638,0.699999999999999);
#4240=CIRCLE('',#10643,0.505000000000001);
#4241=CIRCLE('',#10644,0.505000000000001);
#4242=CIRCLE('',#10646,0.699999999999999);
#4243=CIRCLE('',#10647,0.699999999999999);
#4244=CIRCLE('',#10652,0.225);
#4245=CIRCLE('',#10653,0.225);
#4246=CIRCLE('',#10655,0.800000000000001);
#4247=CIRCLE('',#10656,0.800000000000001);
#4248=CIRCLE('',#10662,0.9);
#4249=CIRCLE('',#10665,0.9);
#4250=CIRCLE('',#10669,1.05);
#4251=CIRCLE('',#10670,0.9);
#4252=CIRCLE('',#10672,1.05);
#4253=CIRCLE('',#10674,1.);
#4254=CIRCLE('',#10676,1.);
#4255=CIRCLE('',#10678,1.05);
#4256=CIRCLE('',#10680,1.05);
#4257=CIRCLE('',#10682,1.);
#4258=CIRCLE('',#10684,1.);
#4259=CIRCLE('',#10686,1.05);
#4260=CIRCLE('',#10688,1.05);
#4261=CIRCLE('',#10690,0.9);
#4262=CIRCLE('',#10694,0.895);
#4263=CIRCLE('',#10695,0.605);
#4264=CIRCLE('',#10698,0.895);
#4265=CIRCLE('',#10699,0.605);
#4266=CIRCLE('',#10702,0.895);
#4267=CIRCLE('',#10703,0.605);
#4268=CIRCLE('',#10705,0.895);
#4269=CIRCLE('',#10707,0.605);
#4270=CIRCLE('',#10721,0.1954);
#4271=CIRCLE('',#10723,0.3);
#4272=CIRCLE('',#10725,0.35);
#4273=CIRCLE('',#10727,0.35);
#4274=CIRCLE('',#10729,0.32);
#4275=CIRCLE('',#10731,0.22);
#4276=CIRCLE('',#10733,0.1954);
#4277=VERTEX_POINT('',#13735);
#4278=VERTEX_POINT('',#13737);
#4279=VERTEX_POINT('',#13741);
#4280=VERTEX_POINT('',#13743);
#4281=VERTEX_POINT('',#13747);
#4282=VERTEX_POINT('',#13749);
#4283=VERTEX_POINT('',#13753);
#4284=VERTEX_POINT('',#13755);
#4285=VERTEX_POINT('',#13759);
#4286=VERTEX_POINT('',#13761);
#4287=VERTEX_POINT('',#13765);
#4288=VERTEX_POINT('',#13767);
#4289=VERTEX_POINT('',#13771);
#4290=VERTEX_POINT('',#13773);
#4291=VERTEX_POINT('',#13777);
#4292=VERTEX_POINT('',#13779);
#4293=VERTEX_POINT('',#13783);
#4294=VERTEX_POINT('',#13785);
#4295=VERTEX_POINT('',#13789);
#4296=VERTEX_POINT('',#13791);
#4297=VERTEX_POINT('',#13795);
#4298=VERTEX_POINT('',#13797);
#4299=VERTEX_POINT('',#13801);
#4300=VERTEX_POINT('',#13803);
#4301=VERTEX_POINT('',#13807);
#4302=VERTEX_POINT('',#13808);
#4303=VERTEX_POINT('',#13810);
#4304=VERTEX_POINT('',#13812);
#4305=VERTEX_POINT('',#13816);
#4306=VERTEX_POINT('',#13818);
#4307=VERTEX_POINT('',#13822);
#4308=VERTEX_POINT('',#13824);
#4309=VERTEX_POINT('',#13834);
#4310=VERTEX_POINT('',#13836);
#4311=VERTEX_POINT('',#13841);
#4312=VERTEX_POINT('',#13843);
#4313=VERTEX_POINT('',#13848);
#4314=VERTEX_POINT('',#13850);
#4315=VERTEX_POINT('',#13854);
#4316=VERTEX_POINT('',#13857);
#4317=VERTEX_POINT('',#13859);
#4318=VERTEX_POINT('',#13863);
#4319=VERTEX_POINT('',#13866);
#4320=VERTEX_POINT('',#13868);
#4321=VERTEX_POINT('',#13872);
#4322=VERTEX_POINT('',#13875);
#4323=VERTEX_POINT('',#13877);
#4324=VERTEX_POINT('',#13881);
#4325=VERTEX_POINT('',#13884);
#4326=VERTEX_POINT('',#13888);
#4327=VERTEX_POINT('',#13892);
#4328=VERTEX_POINT('',#13896);
#4329=VERTEX_POINT('',#13900);
#4330=VERTEX_POINT('',#13901);
#4331=VERTEX_POINT('',#13903);
#4332=VERTEX_POINT('',#13905);
#4333=VERTEX_POINT('',#13909);
#4334=VERTEX_POINT('',#13911);
#4335=VERTEX_POINT('',#13915);
#4336=VERTEX_POINT('',#13917);
#4337=VERTEX_POINT('',#13927);
#4338=VERTEX_POINT('',#13929);
#4339=VERTEX_POINT('',#13933);
#4340=VERTEX_POINT('',#13935);
#4341=VERTEX_POINT('',#13942);
#4342=VERTEX_POINT('',#13944);
#4343=VERTEX_POINT('',#13948);
#4344=VERTEX_POINT('',#13950);
#4345=VERTEX_POINT('',#13957);
#4346=VERTEX_POINT('',#13959);
#4347=VERTEX_POINT('',#13964);
#4348=VERTEX_POINT('',#13966);
#4349=VERTEX_POINT('',#13971);
#4350=VERTEX_POINT('',#13973);
#4351=VERTEX_POINT('',#13977);
#4352=VERTEX_POINT('',#13980);
#4353=VERTEX_POINT('',#13982);
#4354=VERTEX_POINT('',#13986);
#4355=VERTEX_POINT('',#13989);
#4356=VERTEX_POINT('',#13991);
#4357=VERTEX_POINT('',#13995);
#4358=VERTEX_POINT('',#13998);
#4359=VERTEX_POINT('',#14000);
#4360=VERTEX_POINT('',#14004);
#4361=VERTEX_POINT('',#14007);
#4362=VERTEX_POINT('',#14011);
#4363=VERTEX_POINT('',#14015);
#4364=VERTEX_POINT('',#14019);
#4365=VERTEX_POINT('',#14023);
#4366=VERTEX_POINT('',#14024);
#4367=VERTEX_POINT('',#14026);
#4368=VERTEX_POINT('',#14028);
#4369=VERTEX_POINT('',#14032);
#4370=VERTEX_POINT('',#14034);
#4371=VERTEX_POINT('',#14038);
#4372=VERTEX_POINT('',#14040);
#4373=VERTEX_POINT('',#14050);
#4374=VERTEX_POINT('',#14052);
#4375=VERTEX_POINT('',#14056);
#4376=VERTEX_POINT('',#14058);
#4377=VERTEX_POINT('',#14065);
#4378=VERTEX_POINT('',#14067);
#4379=VERTEX_POINT('',#14071);
#4380=VERTEX_POINT('',#14073);
#4381=VERTEX_POINT('',#14080);
#4382=VERTEX_POINT('',#14081);
#4383=VERTEX_POINT('',#14083);
#4384=VERTEX_POINT('',#14085);
#4385=VERTEX_POINT('',#14089);
#4386=VERTEX_POINT('',#14091);
#4387=VERTEX_POINT('',#14096);
#4388=VERTEX_POINT('',#14103);
#4389=VERTEX_POINT('',#14106);
#4390=VERTEX_POINT('',#14108);
#4391=VERTEX_POINT('',#14110);
#4392=VERTEX_POINT('',#14113);
#4393=VERTEX_POINT('',#14116);
#4394=VERTEX_POINT('',#14118);
#4395=VERTEX_POINT('',#14120);
#4396=VERTEX_POINT('',#14122);
#4397=VERTEX_POINT('',#14125);
#4398=VERTEX_POINT('',#14129);
#4399=VERTEX_POINT('',#14133);
#4400=VERTEX_POINT('',#14138);
#4401=VERTEX_POINT('',#14143);
#4402=VERTEX_POINT('',#14148);
#4403=VERTEX_POINT('',#14153);
#4404=VERTEX_POINT('',#14154);
#4405=VERTEX_POINT('',#14159);
#4406=VERTEX_POINT('',#14163);
#4407=VERTEX_POINT('',#14171);
#4408=VERTEX_POINT('',#14172);
#4409=VERTEX_POINT('',#14174);
#4410=VERTEX_POINT('',#14176);
#4411=VERTEX_POINT('',#14180);
#4412=VERTEX_POINT('',#14182);
#4413=VERTEX_POINT('',#14187);
#4414=VERTEX_POINT('',#14194);
#4415=VERTEX_POINT('',#14197);
#4416=VERTEX_POINT('',#14199);
#4417=VERTEX_POINT('',#14201);
#4418=VERTEX_POINT('',#14204);
#4419=VERTEX_POINT('',#14207);
#4420=VERTEX_POINT('',#14209);
#4421=VERTEX_POINT('',#14211);
#4422=VERTEX_POINT('',#14213);
#4423=VERTEX_POINT('',#14216);
#4424=VERTEX_POINT('',#14220);
#4425=VERTEX_POINT('',#14224);
#4426=VERTEX_POINT('',#14229);
#4427=VERTEX_POINT('',#14234);
#4428=VERTEX_POINT('',#14239);
#4429=VERTEX_POINT('',#14244);
#4430=VERTEX_POINT('',#14245);
#4431=VERTEX_POINT('',#14250);
#4432=VERTEX_POINT('',#14254);
#4433=VERTEX_POINT('',#14262);
#4434=VERTEX_POINT('',#14263);
#4435=VERTEX_POINT('',#14265);
#4436=VERTEX_POINT('',#14267);
#4437=VERTEX_POINT('',#14271);
#4438=VERTEX_POINT('',#14273);
#4439=VERTEX_POINT('',#14277);
#4440=VERTEX_POINT('',#14279);
#4441=VERTEX_POINT('',#14289);
#4442=VERTEX_POINT('',#14290);
#4443=VERTEX_POINT('',#14292);
#4444=VERTEX_POINT('',#14294);
#4445=VERTEX_POINT('',#14298);
#4446=VERTEX_POINT('',#14300);
#4447=VERTEX_POINT('',#14304);
#4448=VERTEX_POINT('',#14306);
#4449=VERTEX_POINT('',#14316);
#4450=VERTEX_POINT('',#14319);
#4451=VERTEX_POINT('',#14323);
#4452=VERTEX_POINT('',#14327);
#4453=VERTEX_POINT('',#14331);
#4454=VERTEX_POINT('',#14334);
#4455=VERTEX_POINT('',#14338);
#4456=VERTEX_POINT('',#14342);
#4457=VERTEX_POINT('',#14347);
#4458=VERTEX_POINT('',#14348);
#4459=VERTEX_POINT('',#14350);
#4460=VERTEX_POINT('',#14352);
#4461=VERTEX_POINT('',#14356);
#4462=VERTEX_POINT('',#14358);
#4463=VERTEX_POINT('',#14362);
#4464=VERTEX_POINT('',#14364);
#4465=VERTEX_POINT('',#14368);
#4466=VERTEX_POINT('',#14370);
#4467=VERTEX_POINT('',#14374);
#4468=VERTEX_POINT('',#14376);
#4469=VERTEX_POINT('',#14387);
#4470=VERTEX_POINT('',#14389);
#4471=VERTEX_POINT('',#14393);
#4472=VERTEX_POINT('',#14395);
#4473=VERTEX_POINT('',#14399);
#4474=VERTEX_POINT('',#14400);
#4475=VERTEX_POINT('',#14403);
#4476=VERTEX_POINT('',#14404);
#4477=VERTEX_POINT('',#14406);
#4478=VERTEX_POINT('',#14410);
#4479=VERTEX_POINT('',#14411);
#4480=VERTEX_POINT('',#14413);
#4481=VERTEX_POINT('',#14417);
#4482=VERTEX_POINT('',#14418);
#4483=VERTEX_POINT('',#14420);
#4484=VERTEX_POINT('',#14427);
#4485=VERTEX_POINT('',#14428);
#4486=VERTEX_POINT('',#14430);
#4487=VERTEX_POINT('',#14437);
#4488=VERTEX_POINT('',#14438);
#4489=VERTEX_POINT('',#14440);
#4490=VERTEX_POINT('',#14442);
#4491=VERTEX_POINT('',#14445);
#4492=VERTEX_POINT('',#14447);
#4493=VERTEX_POINT('',#14449);
#4494=VERTEX_POINT('',#14451);
#4495=VERTEX_POINT('',#14454);
#4496=VERTEX_POINT('',#14456);
#4497=VERTEX_POINT('',#14465);
#4498=VERTEX_POINT('',#14466);
#4499=VERTEX_POINT('',#14468);
#4500=VERTEX_POINT('',#14470);
#4501=VERTEX_POINT('',#14474);
#4502=VERTEX_POINT('',#14476);
#4503=VERTEX_POINT('',#14480);
#4504=VERTEX_POINT('',#14482);
#4505=VERTEX_POINT('',#14490);
#4506=VERTEX_POINT('',#14494);
#4507=VERTEX_POINT('',#14498);
#4508=VERTEX_POINT('',#14499);
#4509=VERTEX_POINT('',#14504);
#4510=VERTEX_POINT('',#14508);
#4511=VERTEX_POINT('',#14516);
#4512=VERTEX_POINT('',#14518);
#4513=VERTEX_POINT('',#14522);
#4514=VERTEX_POINT('',#14525);
#4515=VERTEX_POINT('',#14526);
#4516=VERTEX_POINT('',#14528);
#4517=VERTEX_POINT('',#14532);
#4518=VERTEX_POINT('',#14533);
#4519=VERTEX_POINT('',#14544);
#4520=VERTEX_POINT('',#14573);
#4521=VERTEX_POINT('',#14610);
#4522=VERTEX_POINT('',#14645);
#4523=VERTEX_POINT('',#14647);
#4524=VERTEX_POINT('',#14658);
#4525=VERTEX_POINT('',#14688);
#4526=VERTEX_POINT('',#14690);
#4527=VERTEX_POINT('',#14693);
#4528=VERTEX_POINT('',#14694);
#4529=VERTEX_POINT('',#14713);
#4530=VERTEX_POINT('',#14734);
#4531=VERTEX_POINT('',#14735);
#4532=VERTEX_POINT('',#14754);
#4533=VERTEX_POINT('',#14775);
#4534=VERTEX_POINT('',#14776);
#4535=VERTEX_POINT('',#14795);
#4536=VERTEX_POINT('',#14816);
#4537=VERTEX_POINT('',#14817);
#4538=VERTEX_POINT('',#14836);
#4539=VERTEX_POINT('',#14858);
#4540=VERTEX_POINT('',#14895);
#4541=VERTEX_POINT('',#14932);
#4542=VERTEX_POINT('',#14969);
#4543=VERTEX_POINT('',#15006);
#4544=VERTEX_POINT('',#15009);
#4545=VERTEX_POINT('',#15012);
#4546=VERTEX_POINT('',#15016);
#4547=VERTEX_POINT('',#15024);
#4548=VERTEX_POINT('',#15026);
#4549=VERTEX_POINT('',#15030);
#4550=VERTEX_POINT('',#15032);
#4551=VERTEX_POINT('',#15039);
#4552=VERTEX_POINT('',#15040);
#4553=VERTEX_POINT('',#15042);
#4554=VERTEX_POINT('',#15044);
#4555=VERTEX_POINT('',#15048);
#4556=VERTEX_POINT('',#15050);
#4557=VERTEX_POINT('',#15054);
#4558=VERTEX_POINT('',#15056);
#4559=VERTEX_POINT('',#15060);
#4560=VERTEX_POINT('',#15062);
#4561=VERTEX_POINT('',#15066);
#4562=VERTEX_POINT('',#15068);
#4563=VERTEX_POINT('',#15077);
#4564=VERTEX_POINT('',#15080);
#4565=VERTEX_POINT('',#15083);
#4566=VERTEX_POINT('',#15087);
#4567=VERTEX_POINT('',#15091);
#4568=VERTEX_POINT('',#15095);
#4569=VERTEX_POINT('',#15098);
#4570=VERTEX_POINT('',#15105);
#4571=VERTEX_POINT('',#15106);
#4572=VERTEX_POINT('',#15110);
#4573=VERTEX_POINT('',#15112);
#4574=VERTEX_POINT('',#15116);
#4575=VERTEX_POINT('',#15117);
#4576=VERTEX_POINT('',#15119);
#4577=VERTEX_POINT('',#15121);
#4578=VERTEX_POINT('',#15127);
#4579=VERTEX_POINT('',#15129);
#4580=VERTEX_POINT('',#15131);
#4581=VERTEX_POINT('',#15133);
#4582=VERTEX_POINT('',#15136);
#4583=VERTEX_POINT('',#15139);
#4584=VERTEX_POINT('',#15141);
#4585=VERTEX_POINT('',#15144);
#4586=VERTEX_POINT('',#15147);
#4587=VERTEX_POINT('',#15148);
#4588=VERTEX_POINT('',#15150);
#4589=VERTEX_POINT('',#15153);
#4590=VERTEX_POINT('',#15156);
#4591=VERTEX_POINT('',#15159);
#4592=VERTEX_POINT('',#15161);
#4593=VERTEX_POINT('',#15165);
#4594=VERTEX_POINT('',#15169);
#4595=VERTEX_POINT('',#15173);
#4596=VERTEX_POINT('',#15177);
#4597=VERTEX_POINT('',#15179);
#4598=VERTEX_POINT('',#15183);
#4599=VERTEX_POINT('',#15185);
#4600=VERTEX_POINT('',#15188);
#4601=VERTEX_POINT('',#15190);
#4602=VERTEX_POINT('',#15192);
#4603=VERTEX_POINT('',#15194);
#4604=VERTEX_POINT('',#15196);
#4605=VERTEX_POINT('',#15200);
#4606=VERTEX_POINT('',#15204);
#4607=VERTEX_POINT('',#15210);
#4608=VERTEX_POINT('',#15214);
#4609=VERTEX_POINT('',#15218);
#4610=VERTEX_POINT('',#15222);
#4611=VERTEX_POINT('',#15226);
#4612=VERTEX_POINT('',#15234);
#4613=VERTEX_POINT('',#15236);
#4614=VERTEX_POINT('',#15240);
#4615=VERTEX_POINT('',#15244);
#4616=VERTEX_POINT('',#15247);
#4617=VERTEX_POINT('',#15253);
#4618=VERTEX_POINT('',#15254);
#4619=VERTEX_POINT('',#15256);
#4620=VERTEX_POINT('',#15258);
#4621=VERTEX_POINT('',#15262);
#4622=VERTEX_POINT('',#15264);
#4623=VERTEX_POINT('',#15268);
#4624=VERTEX_POINT('',#15270);
#4625=VERTEX_POINT('',#15274);
#4626=VERTEX_POINT('',#15276);
#4627=VERTEX_POINT('',#15280);
#4628=VERTEX_POINT('',#15282);
#4629=VERTEX_POINT('',#15291);
#4630=VERTEX_POINT('',#15294);
#4631=VERTEX_POINT('',#15297);
#4632=VERTEX_POINT('',#15301);
#4633=VERTEX_POINT('',#15305);
#4634=VERTEX_POINT('',#15309);
#4635=VERTEX_POINT('',#15312);
#4636=VERTEX_POINT('',#15319);
#4637=VERTEX_POINT('',#15322);
#4638=VERTEX_POINT('',#15326);
#4639=VERTEX_POINT('',#15330);
#4640=VERTEX_POINT('',#15334);
#4641=VERTEX_POINT('',#15337);
#4642=VERTEX_POINT('',#15341);
#4643=VERTEX_POINT('',#15345);
#4644=VERTEX_POINT('',#15350);
#4645=VERTEX_POINT('',#15351);
#4646=VERTEX_POINT('',#15353);
#4647=VERTEX_POINT('',#15355);
#4648=VERTEX_POINT('',#15359);
#4649=VERTEX_POINT('',#15361);
#4650=VERTEX_POINT('',#15365);
#4651=VERTEX_POINT('',#15367);
#4652=VERTEX_POINT('',#15371);
#4653=VERTEX_POINT('',#15373);
#4654=VERTEX_POINT('',#15377);
#4655=VERTEX_POINT('',#15379);
#4656=VERTEX_POINT('',#15389);
#4657=VERTEX_POINT('',#15392);
#4658=VERTEX_POINT('',#15394);
#4659=VERTEX_POINT('',#15403);
#4660=VERTEX_POINT('',#15404);
#4661=VERTEX_POINT('',#15406);
#4662=VERTEX_POINT('',#15408);
#4663=VERTEX_POINT('',#15412);
#4664=VERTEX_POINT('',#15414);
#4665=VERTEX_POINT('',#15418);
#4666=VERTEX_POINT('',#15420);
#4667=VERTEX_POINT('',#15426);
#4668=VERTEX_POINT('',#15428);
#4669=VERTEX_POINT('',#15436);
#4670=VERTEX_POINT('',#15437);
#4671=VERTEX_POINT('',#15441);
#4672=VERTEX_POINT('',#15456);
#4673=VERTEX_POINT('',#15458);
#4674=VERTEX_POINT('',#15460);
#4675=VERTEX_POINT('',#15497);
#4676=VERTEX_POINT('',#15516);
#4677=VERTEX_POINT('',#15518);
#4678=VERTEX_POINT('',#15522);
#4679=VERTEX_POINT('',#15524);
#4680=VERTEX_POINT('',#15531);
#4681=VERTEX_POINT('',#15532);
#4682=VERTEX_POINT('',#15536);
#4683=VERTEX_POINT('',#15551);
#4684=VERTEX_POINT('',#15553);
#4685=VERTEX_POINT('',#15555);
#4686=VERTEX_POINT('',#15592);
#4687=VERTEX_POINT('',#15611);
#4688=VERTEX_POINT('',#15613);
#4689=VERTEX_POINT('',#15617);
#4690=VERTEX_POINT('',#15619);
#4691=VERTEX_POINT('',#15626);
#4692=VERTEX_POINT('',#15628);
#4693=VERTEX_POINT('',#15632);
#4694=VERTEX_POINT('',#15634);
#4695=VERTEX_POINT('',#15641);
#4696=VERTEX_POINT('',#15642);
#4697=VERTEX_POINT('',#15644);
#4698=VERTEX_POINT('',#15646);
#4699=VERTEX_POINT('',#15651);
#4700=VERTEX_POINT('',#15652);
#4701=VERTEX_POINT('',#15654);
#4702=VERTEX_POINT('',#15656);
#4703=VERTEX_POINT('',#15660);
#4704=VERTEX_POINT('',#15662);
#4705=VERTEX_POINT('',#15667);
#4706=VERTEX_POINT('',#15668);
#4707=VERTEX_POINT('',#15672);
#4708=VERTEX_POINT('',#15683);
#4709=VERTEX_POINT('',#15685);
#4710=VERTEX_POINT('',#15692);
#4711=VERTEX_POINT('',#15694);
#4712=VERTEX_POINT('',#15730);
#4713=VERTEX_POINT('',#15741);
#4714=VERTEX_POINT('',#15744);
#4715=VERTEX_POINT('',#15748);
#4716=VERTEX_POINT('',#15752);
#4717=VERTEX_POINT('',#15758);
#4718=VERTEX_POINT('',#15762);
#4719=VERTEX_POINT('',#15764);
#4720=VERTEX_POINT('',#15769);
#4721=VERTEX_POINT('',#15777);
#4722=VERTEX_POINT('',#15779);
#4723=VERTEX_POINT('',#15784);
#4724=VERTEX_POINT('',#15786);
#4725=VERTEX_POINT('',#15789);
#4726=VERTEX_POINT('',#15794);
#4727=VERTEX_POINT('',#15800);
#4728=VERTEX_POINT('',#15802);
#4729=VERTEX_POINT('',#15806);
#4730=VERTEX_POINT('',#15808);
#4731=VERTEX_POINT('',#15815);
#4732=VERTEX_POINT('',#15817);
#4733=VERTEX_POINT('',#15821);
#4734=VERTEX_POINT('',#15823);
#4735=VERTEX_POINT('',#15830);
#4736=VERTEX_POINT('',#15832);
#4737=VERTEX_POINT('',#15836);
#4738=VERTEX_POINT('',#15838);
#4739=VERTEX_POINT('',#15845);
#4740=VERTEX_POINT('',#15846);
#4741=VERTEX_POINT('',#15848);
#4742=VERTEX_POINT('',#15850);
#4743=VERTEX_POINT('',#15852);
#4744=VERTEX_POINT('',#15854);
#4745=VERTEX_POINT('',#15856);
#4746=VERTEX_POINT('',#15858);
#4747=VERTEX_POINT('',#15862);
#4748=VERTEX_POINT('',#15864);
#4749=VERTEX_POINT('',#15868);
#4750=VERTEX_POINT('',#15872);
#4751=VERTEX_POINT('',#15876);
#4752=VERTEX_POINT('',#15880);
#4753=VERTEX_POINT('',#15881);
#4754=VERTEX_POINT('',#15884);
#4755=VERTEX_POINT('',#15896);
#4756=VERTEX_POINT('',#15897);
#4757=VERTEX_POINT('',#15899);
#4758=VERTEX_POINT('',#15901);
#4759=VERTEX_POINT('',#15905);
#4760=VERTEX_POINT('',#15907);
#4761=VERTEX_POINT('',#15911);
#4762=VERTEX_POINT('',#15913);
#4763=VERTEX_POINT('',#15917);
#4764=VERTEX_POINT('',#15919);
#4765=VERTEX_POINT('',#15923);
#4766=VERTEX_POINT('',#15925);
#4767=VERTEX_POINT('',#15933);
#4768=VERTEX_POINT('',#15936);
#4769=VERTEX_POINT('',#15940);
#4770=VERTEX_POINT('',#15944);
#4771=VERTEX_POINT('',#15951);
#4772=VERTEX_POINT('',#15953);
#4773=VERTEX_POINT('',#15957);
#4774=VERTEX_POINT('',#15959);
#4775=VERTEX_POINT('',#15963);
#4776=VERTEX_POINT('',#15964);
#4777=VERTEX_POINT('',#15966);
#4778=VERTEX_POINT('',#15968);
#4779=VERTEX_POINT('',#15972);
#4780=VERTEX_POINT('',#15974);
#4781=VERTEX_POINT('',#15978);
#4782=VERTEX_POINT('',#15982);
#4783=VERTEX_POINT('',#15990);
#4784=VERTEX_POINT('',#15992);
#4785=VERTEX_POINT('',#15996);
#4786=VERTEX_POINT('',#15998);
#4787=VERTEX_POINT('',#16005);
#4788=VERTEX_POINT('',#16007);
#4789=VERTEX_POINT('',#16011);
#4790=VERTEX_POINT('',#16013);
#4791=VERTEX_POINT('',#16020);
#4792=VERTEX_POINT('',#16022);
#4793=VERTEX_POINT('',#16026);
#4794=VERTEX_POINT('',#16028);
#4795=VERTEX_POINT('',#16035);
#4796=VERTEX_POINT('',#16037);
#4797=VERTEX_POINT('',#16041);
#4798=VERTEX_POINT('',#16043);
#4799=VERTEX_POINT('',#16051);
#4800=VERTEX_POINT('',#16052);
#4801=VERTEX_POINT('',#16055);
#4802=VERTEX_POINT('',#16057);
#4803=VERTEX_POINT('',#16061);
#4804=VERTEX_POINT('',#16065);
#4805=VERTEX_POINT('',#16067);
#4806=VERTEX_POINT('',#16071);
#4807=VERTEX_POINT('',#16076);
#4808=VERTEX_POINT('',#16080);
#4809=VERTEX_POINT('',#16086);
#4810=VERTEX_POINT('',#16087);
#4811=VERTEX_POINT('',#16090);
#4812=VERTEX_POINT('',#16092);
#4813=VERTEX_POINT('',#16096);
#4814=VERTEX_POINT('',#16100);
#4815=VERTEX_POINT('',#16102);
#4816=VERTEX_POINT('',#16105);
#4817=VERTEX_POINT('',#16109);
#4818=VERTEX_POINT('',#16113);
#4819=VERTEX_POINT('',#16121);
#4820=VERTEX_POINT('',#16122);
#4821=VERTEX_POINT('',#16125);
#4822=VERTEX_POINT('',#16126);
#4823=VERTEX_POINT('',#16129);
#4824=VERTEX_POINT('',#16130);
#4825=VERTEX_POINT('',#16133);
#4826=VERTEX_POINT('',#16134);
#4827=VERTEX_POINT('',#16137);
#4828=VERTEX_POINT('',#16138);
#4829=VERTEX_POINT('',#16141);
#4830=VERTEX_POINT('',#16142);
#4831=VERTEX_POINT('',#16145);
#4832=VERTEX_POINT('',#16146);
#4833=VERTEX_POINT('',#16149);
#4834=VERTEX_POINT('',#16150);
#4835=VERTEX_POINT('',#16154);
#4836=VERTEX_POINT('',#16155);
#4837=VERTEX_POINT('',#16178);
#4838=VERTEX_POINT('',#16180);
#4839=VERTEX_POINT('',#16205);
#4840=VERTEX_POINT('',#16207);
#4841=VERTEX_POINT('',#16230);
#4842=VERTEX_POINT('',#16232);
#4843=VERTEX_POINT('',#16255);
#4844=VERTEX_POINT('',#16257);
#4845=VERTEX_POINT('',#16270);
#4846=VERTEX_POINT('',#16273);
#4847=VERTEX_POINT('',#16286);
#4848=VERTEX_POINT('',#16288);
#4849=VERTEX_POINT('',#16311);
#4850=VERTEX_POINT('',#16313);
#4851=VERTEX_POINT('',#16336);
#4852=VERTEX_POINT('',#16338);
#4853=VERTEX_POINT('',#16361);
#4854=VERTEX_POINT('',#16363);
#4855=VERTEX_POINT('',#16388);
#4856=VERTEX_POINT('',#16392);
#4857=VERTEX_POINT('',#16417);
#4858=VERTEX_POINT('',#16421);
#4859=VERTEX_POINT('',#16446);
#4860=VERTEX_POINT('',#16450);
#4861=VERTEX_POINT('',#16451);
#4862=VERTEX_POINT('',#16478);
#4863=VERTEX_POINT('',#16482);
#4864=VERTEX_POINT('',#16507);
#4865=VERTEX_POINT('',#16511);
#4866=VERTEX_POINT('',#16536);
#4867=VERTEX_POINT('',#16540);
#4868=VERTEX_POINT('',#16565);
#4869=VERTEX_POINT('',#16568);
#4870=VERTEX_POINT('',#16570);
#4871=VERTEX_POINT('',#16602);
#4872=VERTEX_POINT('',#16604);
#4873=VERTEX_POINT('',#16607);
#4874=VERTEX_POINT('',#16611);
#4875=VERTEX_POINT('',#16616);
#4876=VERTEX_POINT('',#16618);
#4877=VERTEX_POINT('',#16621);
#4878=VERTEX_POINT('',#16625);
#4879=VERTEX_POINT('',#16644);
#4880=VERTEX_POINT('',#16646);
#4881=VERTEX_POINT('',#16650);
#4882=VERTEX_POINT('',#16651);
#4883=VERTEX_POINT('',#16653);
#4884=VERTEX_POINT('',#16655);
#4885=VERTEX_POINT('',#16659);
#4886=VERTEX_POINT('',#16661);
#4887=VERTEX_POINT('',#16665);
#4888=VERTEX_POINT('',#16667);
#4889=VERTEX_POINT('',#16675);
#4890=VERTEX_POINT('',#16677);
#4891=VERTEX_POINT('',#16681);
#4892=VERTEX_POINT('',#16683);
#4893=VERTEX_POINT('',#16687);
#4894=VERTEX_POINT('',#16689);
#4895=VERTEX_POINT('',#16693);
#4896=VERTEX_POINT('',#16695);
#4897=VERTEX_POINT('',#16699);
#4898=VERTEX_POINT('',#16701);
#4899=VERTEX_POINT('',#16705);
#4900=VERTEX_POINT('',#16707);
#4901=VERTEX_POINT('',#16711);
#4902=VERTEX_POINT('',#16712);
#4903=VERTEX_POINT('',#16714);
#4904=VERTEX_POINT('',#16716);
#4905=VERTEX_POINT('',#16720);
#4906=VERTEX_POINT('',#16722);
#4907=VERTEX_POINT('',#16726);
#4908=VERTEX_POINT('',#16728);
#4909=VERTEX_POINT('',#16738);
#4910=VERTEX_POINT('',#16740);
#4911=VERTEX_POINT('',#16744);
#4912=VERTEX_POINT('',#16746);
#4913=VERTEX_POINT('',#16750);
#4914=VERTEX_POINT('',#16752);
#4915=VERTEX_POINT('',#16756);
#4916=VERTEX_POINT('',#16758);
#4917=VERTEX_POINT('',#16762);
#4918=VERTEX_POINT('',#16764);
#4919=VERTEX_POINT('',#16768);
#4920=VERTEX_POINT('',#16770);
#4921=VERTEX_POINT('',#16774);
#4922=VERTEX_POINT('',#16775);
#4923=VERTEX_POINT('',#16777);
#4924=VERTEX_POINT('',#16779);
#4925=VERTEX_POINT('',#16783);
#4926=VERTEX_POINT('',#16785);
#4927=VERTEX_POINT('',#16789);
#4928=VERTEX_POINT('',#16791);
#4929=VERTEX_POINT('',#16801);
#4930=VERTEX_POINT('',#16803);
#4931=VERTEX_POINT('',#16807);
#4932=VERTEX_POINT('',#16809);
#4933=VERTEX_POINT('',#16813);
#4934=VERTEX_POINT('',#16815);
#4935=VERTEX_POINT('',#16819);
#4936=VERTEX_POINT('',#16821);
#4937=VERTEX_POINT('',#16825);
#4938=VERTEX_POINT('',#16827);
#4939=VERTEX_POINT('',#16831);
#4940=VERTEX_POINT('',#16833);
#4941=VERTEX_POINT('',#16837);
#4942=VERTEX_POINT('',#16838);
#4943=VERTEX_POINT('',#16840);
#4944=VERTEX_POINT('',#16842);
#4945=VERTEX_POINT('',#16846);
#4946=VERTEX_POINT('',#16848);
#4947=VERTEX_POINT('',#16852);
#4948=VERTEX_POINT('',#16854);
#4949=VERTEX_POINT('',#16864);
#4950=VERTEX_POINT('',#16866);
#4951=VERTEX_POINT('',#16871);
#4952=VERTEX_POINT('',#16873);
#4953=VERTEX_POINT('',#16876);
#4954=VERTEX_POINT('',#16881);
#4955=VERTEX_POINT('',#16887);
#4956=VERTEX_POINT('',#16889);
#4957=VERTEX_POINT('',#16893);
#4958=VERTEX_POINT('',#16895);
#4959=VERTEX_POINT('',#16902);
#4960=VERTEX_POINT('',#16904);
#4961=VERTEX_POINT('',#16908);
#4962=VERTEX_POINT('',#16910);
#4963=VERTEX_POINT('',#16917);
#4964=VERTEX_POINT('',#16919);
#4965=VERTEX_POINT('',#16923);
#4966=VERTEX_POINT('',#16925);
#4967=VERTEX_POINT('',#16933);
#4968=VERTEX_POINT('',#16934);
#4969=VERTEX_POINT('',#16936);
#4970=VERTEX_POINT('',#16938);
#4971=VERTEX_POINT('',#16942);
#4972=VERTEX_POINT('',#16944);
#4973=VERTEX_POINT('',#16948);
#4974=VERTEX_POINT('',#16950);
#4975=VERTEX_POINT('',#16958);
#4976=VERTEX_POINT('',#16960);
#4977=VERTEX_POINT('',#16963);
#4978=VERTEX_POINT('',#16967);
#4979=VERTEX_POINT('',#16970);
#4980=VERTEX_POINT('',#16974);
#4981=VERTEX_POINT('',#16977);
#4982=VERTEX_POINT('',#16981);
#4983=VERTEX_POINT('',#16984);
#4984=VERTEX_POINT('',#16988);
#4985=VERTEX_POINT('',#16991);
#4986=VERTEX_POINT('',#16995);
#4987=VERTEX_POINT('',#17001);
#4988=VERTEX_POINT('',#17002);
#4989=VERTEX_POINT('',#17004);
#4990=VERTEX_POINT('',#17006);
#4991=VERTEX_POINT('',#17010);
#4992=VERTEX_POINT('',#17012);
#4993=VERTEX_POINT('',#17016);
#4994=VERTEX_POINT('',#17018);
#4995=VERTEX_POINT('',#17025);
#4996=VERTEX_POINT('',#17027);
#4997=VERTEX_POINT('',#17030);
#4998=VERTEX_POINT('',#17034);
#4999=VERTEX_POINT('',#17042);
#5000=VERTEX_POINT('',#17043);
#5001=VERTEX_POINT('',#17045);
#5002=VERTEX_POINT('',#17047);
#5003=VERTEX_POINT('',#17051);
#5004=VERTEX_POINT('',#17053);
#5005=VERTEX_POINT('',#17057);
#5006=VERTEX_POINT('',#17059);
#5007=VERTEX_POINT('',#17063);
#5008=VERTEX_POINT('',#17065);
#5009=VERTEX_POINT('',#17069);
#5010=VERTEX_POINT('',#17071);
#5011=VERTEX_POINT('',#17080);
#5012=VERTEX_POINT('',#17083);
#5013=VERTEX_POINT('',#17086);
#5014=VERTEX_POINT('',#17090);
#5015=VERTEX_POINT('',#17094);
#5016=VERTEX_POINT('',#17098);
#5017=VERTEX_POINT('',#17101);
#5018=EDGE_CURVE('',#4277,#4277,#3838,.T.);
#5019=EDGE_CURVE('',#4277,#4278,#2616,.T.);
#5020=EDGE_CURVE('',#4278,#4278,#3839,.T.);
#5021=EDGE_CURVE('',#4279,#4279,#3840,.T.);
#5022=EDGE_CURVE('',#4279,#4280,#2617,.T.);
#5023=EDGE_CURVE('',#4280,#4280,#3841,.T.);
#5024=EDGE_CURVE('',#4281,#4281,#3842,.T.);
#5025=EDGE_CURVE('',#4281,#4282,#2618,.T.);
#5026=EDGE_CURVE('',#4282,#4282,#3843,.T.);
#5027=EDGE_CURVE('',#4283,#4283,#3844,.T.);
#5028=EDGE_CURVE('',#4283,#4284,#2619,.T.);
#5029=EDGE_CURVE('',#4284,#4284,#3845,.T.);
#5030=EDGE_CURVE('',#4285,#4285,#3846,.T.);
#5031=EDGE_CURVE('',#4285,#4286,#2620,.T.);
#5032=EDGE_CURVE('',#4286,#4286,#3847,.T.);
#5033=EDGE_CURVE('',#4287,#4287,#3848,.T.);
#5034=EDGE_CURVE('',#4287,#4288,#2621,.T.);
#5035=EDGE_CURVE('',#4288,#4288,#3849,.T.);
#5036=EDGE_CURVE('',#4289,#4289,#3850,.T.);
#5037=EDGE_CURVE('',#4289,#4290,#2622,.T.);
#5038=EDGE_CURVE('',#4290,#4290,#3851,.T.);
#5039=EDGE_CURVE('',#4291,#4291,#3852,.T.);
#5040=EDGE_CURVE('',#4291,#4292,#2623,.T.);
#5041=EDGE_CURVE('',#4292,#4292,#3853,.T.);
#5042=EDGE_CURVE('',#4293,#4293,#3854,.T.);
#5043=EDGE_CURVE('',#4293,#4294,#2624,.T.);
#5044=EDGE_CURVE('',#4294,#4294,#3855,.T.);
#5045=EDGE_CURVE('',#4295,#4295,#3856,.T.);
#5046=EDGE_CURVE('',#4295,#4296,#2625,.T.);
#5047=EDGE_CURVE('',#4296,#4296,#3857,.T.);
#5048=EDGE_CURVE('',#4297,#4297,#3858,.T.);
#5049=EDGE_CURVE('',#4297,#4298,#2626,.T.);
#5050=EDGE_CURVE('',#4298,#4298,#3859,.T.);
#5051=EDGE_CURVE('',#4299,#4299,#3860,.T.);
#5052=EDGE_CURVE('',#4299,#4300,#2627,.T.);
#5053=EDGE_CURVE('',#4300,#4300,#3861,.T.);
#5054=EDGE_CURVE('',#4301,#4302,#2628,.T.);
#5055=EDGE_CURVE('',#4302,#4303,#2629,.T.);
#5056=EDGE_CURVE('',#4304,#4303,#2630,.T.);
#5057=EDGE_CURVE('',#4301,#4304,#2631,.T.);
#5058=EDGE_CURVE('',#4305,#4301,#2632,.T.);
#5059=EDGE_CURVE('',#4306,#4304,#2633,.T.);
#5060=EDGE_CURVE('',#4305,#4306,#2634,.T.);
#5061=EDGE_CURVE('',#4307,#4305,#2635,.T.);
#5062=EDGE_CURVE('',#4308,#4306,#2636,.T.);
#5063=EDGE_CURVE('',#4307,#4308,#2637,.T.);
#5064=EDGE_CURVE('',#4302,#4307,#2638,.T.);
#5065=EDGE_CURVE('',#4303,#4308,#2639,.T.);
#5066=EDGE_CURVE('',#4309,#4309,#3862,.T.);
#5067=EDGE_CURVE('',#4309,#4310,#2640,.T.);
#5068=EDGE_CURVE('',#4310,#4310,#3863,.T.);
#5069=EDGE_CURVE('',#4311,#4311,#3864,.T.);
#5070=EDGE_CURVE('',#4311,#4312,#2641,.T.);
#5071=EDGE_CURVE('',#4312,#4312,#3865,.T.);
#5072=EDGE_CURVE('',#4313,#4313,#3866,.T.);
#5073=EDGE_CURVE('',#4313,#4314,#2642,.T.);
#5074=EDGE_CURVE('',#4314,#4314,#3867,.T.);
#5075=EDGE_CURVE('',#4315,#4315,#3868,.T.);
#5076=EDGE_CURVE('',#4316,#4316,#3869,.T.);
#5077=EDGE_CURVE('',#4316,#4317,#2643,.T.);
#5078=EDGE_CURVE('',#4317,#4317,#3870,.T.);
#5079=EDGE_CURVE('',#4318,#4318,#3871,.T.);
#5080=EDGE_CURVE('',#4319,#4319,#3872,.T.);
#5081=EDGE_CURVE('',#4319,#4320,#2644,.T.);
#5082=EDGE_CURVE('',#4320,#4320,#3873,.T.);
#5083=EDGE_CURVE('',#4321,#4321,#3874,.T.);
#5084=EDGE_CURVE('',#4322,#4322,#3875,.T.);
#5085=EDGE_CURVE('',#4322,#4323,#2645,.T.);
#5086=EDGE_CURVE('',#4323,#4323,#3876,.T.);
#5087=EDGE_CURVE('',#4324,#4324,#3877,.T.);
#5088=EDGE_CURVE('',#4325,#4325,#3878,.T.);
#5089=EDGE_CURVE('',#4325,#4315,#2646,.T.);
#5090=EDGE_CURVE('',#4326,#4326,#3879,.T.);
#5091=EDGE_CURVE('',#4326,#4318,#2647,.T.);
#5092=EDGE_CURVE('',#4327,#4327,#3880,.T.);
#5093=EDGE_CURVE('',#4327,#4321,#2648,.T.);
#5094=EDGE_CURVE('',#4328,#4328,#3881,.T.);
#5095=EDGE_CURVE('',#4328,#4324,#2649,.T.);
#5096=EDGE_CURVE('',#4329,#4330,#2650,.T.);
#5097=EDGE_CURVE('',#4330,#4331,#2651,.T.);
#5098=EDGE_CURVE('',#4332,#4331,#2652,.T.);
#5099=EDGE_CURVE('',#4329,#4332,#2653,.T.);
#5100=EDGE_CURVE('',#4333,#4329,#2654,.T.);
#5101=EDGE_CURVE('',#4334,#4332,#2655,.T.);
#5102=EDGE_CURVE('',#4333,#4334,#2656,.T.);
#5103=EDGE_CURVE('',#4335,#4333,#2657,.T.);
#5104=EDGE_CURVE('',#4336,#4334,#2658,.T.);
#5105=EDGE_CURVE('',#4335,#4336,#2659,.T.);
#5106=EDGE_CURVE('',#4330,#4335,#2660,.T.);
#5107=EDGE_CURVE('',#4331,#4336,#2661,.T.);
#5108=EDGE_CURVE('',#4337,#4337,#3882,.T.);
#5109=EDGE_CURVE('',#4337,#4338,#2662,.T.);
#5110=EDGE_CURVE('',#4338,#4338,#3883,.T.);
#5111=EDGE_CURVE('',#4339,#4339,#3884,.T.);
#5112=EDGE_CURVE('',#4339,#4340,#2663,.T.);
#5113=EDGE_CURVE('',#4340,#4340,#3885,.T.);
#5114=EDGE_CURVE('',#4341,#4341,#3886,.T.);
#5115=EDGE_CURVE('',#4341,#4342,#2664,.T.);
#5116=EDGE_CURVE('',#4342,#4342,#3887,.T.);
#5117=EDGE_CURVE('',#4343,#4343,#3888,.T.);
#5118=EDGE_CURVE('',#4343,#4344,#2665,.T.);
#5119=EDGE_CURVE('',#4344,#4344,#3889,.T.);
#5120=EDGE_CURVE('',#4345,#4345,#3890,.T.);
#5121=EDGE_CURVE('',#4345,#4346,#2666,.T.);
#5122=EDGE_CURVE('',#4346,#4346,#3891,.T.);
#5123=EDGE_CURVE('',#4347,#4347,#3892,.T.);
#5124=EDGE_CURVE('',#4347,#4348,#2667,.T.);
#5125=EDGE_CURVE('',#4348,#4348,#3893,.T.);
#5126=EDGE_CURVE('',#4349,#4349,#3894,.T.);
#5127=EDGE_CURVE('',#4349,#4350,#2668,.T.);
#5128=EDGE_CURVE('',#4350,#4350,#3895,.T.);
#5129=EDGE_CURVE('',#4351,#4351,#3896,.T.);
#5130=EDGE_CURVE('',#4352,#4352,#3897,.T.);
#5131=EDGE_CURVE('',#4352,#4353,#2669,.T.);
#5132=EDGE_CURVE('',#4353,#4353,#3898,.T.);
#5133=EDGE_CURVE('',#4354,#4354,#3899,.T.);
#5134=EDGE_CURVE('',#4355,#4355,#3900,.T.);
#5135=EDGE_CURVE('',#4355,#4356,#2670,.T.);
#5136=EDGE_CURVE('',#4356,#4356,#3901,.T.);
#5137=EDGE_CURVE('',#4357,#4357,#3902,.T.);
#5138=EDGE_CURVE('',#4358,#4358,#3903,.T.);
#5139=EDGE_CURVE('',#4358,#4359,#2671,.T.);
#5140=EDGE_CURVE('',#4359,#4359,#3904,.T.);
#5141=EDGE_CURVE('',#4360,#4360,#3905,.T.);
#5142=EDGE_CURVE('',#4361,#4361,#3906,.T.);
#5143=EDGE_CURVE('',#4361,#4351,#2672,.T.);
#5144=EDGE_CURVE('',#4362,#4362,#3907,.T.);
#5145=EDGE_CURVE('',#4362,#4354,#2673,.T.);
#5146=EDGE_CURVE('',#4363,#4363,#3908,.T.);
#5147=EDGE_CURVE('',#4363,#4357,#2674,.T.);
#5148=EDGE_CURVE('',#4364,#4364,#3909,.T.);
#5149=EDGE_CURVE('',#4364,#4360,#2675,.T.);
#5150=EDGE_CURVE('',#4365,#4366,#2676,.T.);
#5151=EDGE_CURVE('',#4366,#4367,#2677,.T.);
#5152=EDGE_CURVE('',#4368,#4367,#2678,.T.);
#5153=EDGE_CURVE('',#4365,#4368,#2679,.T.);
#5154=EDGE_CURVE('',#4369,#4365,#2680,.T.);
#5155=EDGE_CURVE('',#4370,#4368,#2681,.T.);
#5156=EDGE_CURVE('',#4369,#4370,#2682,.T.);
#5157=EDGE_CURVE('',#4371,#4369,#2683,.T.);
#5158=EDGE_CURVE('',#4372,#4370,#2684,.T.);
#5159=EDGE_CURVE('',#4371,#4372,#2685,.T.);
#5160=EDGE_CURVE('',#4366,#4371,#2686,.T.);
#5161=EDGE_CURVE('',#4367,#4372,#2687,.T.);
#5162=EDGE_CURVE('',#4373,#4373,#3910,.T.);
#5163=EDGE_CURVE('',#4373,#4374,#2688,.T.);
#5164=EDGE_CURVE('',#4374,#4374,#3911,.T.);
#5165=EDGE_CURVE('',#4375,#4375,#3912,.T.);
#5166=EDGE_CURVE('',#4375,#4376,#2689,.T.);
#5167=EDGE_CURVE('',#4376,#4376,#3913,.T.);
#5168=EDGE_CURVE('',#4377,#4377,#3914,.T.);
#5169=EDGE_CURVE('',#4377,#4378,#2690,.T.);
#5170=EDGE_CURVE('',#4378,#4378,#3915,.T.);
#5171=EDGE_CURVE('',#4379,#4379,#3916,.T.);
#5172=EDGE_CURVE('',#4379,#4380,#2691,.T.);
#5173=EDGE_CURVE('',#4380,#4380,#3917,.T.);
#5174=EDGE_CURVE('',#4381,#4382,#2692,.T.);
#5175=EDGE_CURVE('',#4383,#4381,#3918,.T.);
#5176=EDGE_CURVE('',#4383,#4384,#2693,.T.);
#5177=EDGE_CURVE('',#4382,#4384,#3919,.T.);
#5178=EDGE_CURVE('',#4385,#4385,#3920,.T.);
#5179=EDGE_CURVE('',#4385,#4386,#2694,.T.);
#5180=EDGE_CURVE('',#4386,#4386,#3921,.T.);
#5181=EDGE_CURVE('',#4385,#4386,#2695,.T.);
#5182=EDGE_CURVE('',#4387,#4387,#3922,.T.);
#5183=EDGE_CURVE('',#4384,#4382,#3923,.T.);
#5184=EDGE_CURVE('',#4383,#4384,#2696,.T.);
#5185=EDGE_CURVE('',#4381,#4383,#3924,.T.);
#5186=EDGE_CURVE('',#4388,#4388,#3925,.T.);
#5187=EDGE_CURVE('',#4389,#4386,#2697,.T.);
#5188=EDGE_CURVE('',#4386,#4390,#2698,.T.);
#5189=EDGE_CURVE('',#4390,#4391,#2699,.T.);
#5190=EDGE_CURVE('',#4391,#4384,#2700,.T.);
#5191=EDGE_CURVE('',#4384,#4392,#2701,.T.);
#5192=EDGE_CURVE('',#4392,#4389,#2702,.T.);
#5193=EDGE_CURVE('',#4393,#4393,#3926,.T.);
#5194=EDGE_CURVE('',#4394,#4394,#3927,.T.);
#5195=EDGE_CURVE('',#4395,#4395,#3928,.T.);
#5196=EDGE_CURVE('',#4396,#4396,#3929,.T.);
#5197=EDGE_CURVE('',#4397,#4397,#3930,.T.);
#5198=EDGE_CURVE('',#4397,#4387,#2703,.T.);
#5199=EDGE_CURVE('',#4398,#4398,#3931,.T.);
#5200=EDGE_CURVE('',#4398,#4388,#2704,.T.);
#5201=EDGE_CURVE('',#4399,#4399,#3932,.T.);
#5202=EDGE_CURVE('',#4399,#4396,#2705,.T.);
#5203=EDGE_CURVE('',#4400,#4400,#3933,.T.);
#5204=EDGE_CURVE('',#4400,#4395,#2706,.T.);
#5205=EDGE_CURVE('',#4401,#4401,#3934,.T.);
#5206=EDGE_CURVE('',#4401,#4394,#2707,.T.);
#5207=EDGE_CURVE('',#4402,#4402,#3935,.T.);
#5208=EDGE_CURVE('',#4402,#4393,#2708,.T.);
#5209=EDGE_CURVE('',#4403,#4404,#2709,.T.);
#5210=EDGE_CURVE('',#4404,#4389,#2710,.T.);
#5211=EDGE_CURVE('',#4403,#4392,#2711,.T.);
#5212=EDGE_CURVE('',#4405,#4403,#2712,.T.);
#5213=EDGE_CURVE('',#4405,#4391,#2713,.T.);
#5214=EDGE_CURVE('',#4406,#4405,#2714,.T.);
#5215=EDGE_CURVE('',#4406,#4390,#2715,.T.);
#5216=EDGE_CURVE('',#4404,#4406,#2716,.T.);
#5217=EDGE_CURVE('',#4407,#4408,#2717,.T.);
#5218=EDGE_CURVE('',#4409,#4407,#3936,.T.);
#5219=EDGE_CURVE('',#4409,#4410,#2718,.T.);
#5220=EDGE_CURVE('',#4408,#4410,#3937,.T.);
#5221=EDGE_CURVE('',#4411,#4411,#3938,.T.);
#5222=EDGE_CURVE('',#4411,#4412,#2719,.T.);
#5223=EDGE_CURVE('',#4412,#4412,#3939,.T.);
#5224=EDGE_CURVE('',#4411,#4412,#2720,.T.);
#5225=EDGE_CURVE('',#4413,#4413,#3940,.T.);
#5226=EDGE_CURVE('',#4410,#4408,#3941,.T.);
#5227=EDGE_CURVE('',#4409,#4410,#2721,.T.);
#5228=EDGE_CURVE('',#4407,#4409,#3942,.T.);
#5229=EDGE_CURVE('',#4414,#4414,#3943,.T.);
#5230=EDGE_CURVE('',#4415,#4412,#2722,.T.);
#5231=EDGE_CURVE('',#4412,#4416,#2723,.T.);
#5232=EDGE_CURVE('',#4416,#4417,#2724,.T.);
#5233=EDGE_CURVE('',#4417,#4410,#2725,.T.);
#5234=EDGE_CURVE('',#4410,#4418,#2726,.T.);
#5235=EDGE_CURVE('',#4418,#4415,#2727,.T.);
#5236=EDGE_CURVE('',#4419,#4419,#3944,.T.);
#5237=EDGE_CURVE('',#4420,#4420,#3945,.T.);
#5238=EDGE_CURVE('',#4421,#4421,#3946,.T.);
#5239=EDGE_CURVE('',#4422,#4422,#3947,.T.);
#5240=EDGE_CURVE('',#4423,#4423,#3948,.T.);
#5241=EDGE_CURVE('',#4423,#4413,#2728,.T.);
#5242=EDGE_CURVE('',#4424,#4424,#3949,.T.);
#5243=EDGE_CURVE('',#4424,#4414,#2729,.T.);
#5244=EDGE_CURVE('',#4425,#4425,#3950,.T.);
#5245=EDGE_CURVE('',#4425,#4422,#2730,.T.);
#5246=EDGE_CURVE('',#4426,#4426,#3951,.T.);
#5247=EDGE_CURVE('',#4426,#4421,#2731,.T.);
#5248=EDGE_CURVE('',#4427,#4427,#3952,.T.);
#5249=EDGE_CURVE('',#4427,#4420,#2732,.T.);
#5250=EDGE_CURVE('',#4428,#4428,#3953,.T.);
#5251=EDGE_CURVE('',#4428,#4419,#2733,.T.);
#5252=EDGE_CURVE('',#4429,#4430,#2734,.T.);
#5253=EDGE_CURVE('',#4430,#4415,#2735,.T.);
#5254=EDGE_CURVE('',#4429,#4418,#2736,.T.);
#5255=EDGE_CURVE('',#4431,#4429,#2737,.T.);
#5256=EDGE_CURVE('',#4431,#4417,#2738,.T.);
#5257=EDGE_CURVE('',#4432,#4431,#2739,.T.);
#5258=EDGE_CURVE('',#4432,#4416,#2740,.T.);
#5259=EDGE_CURVE('',#4430,#4432,#2741,.T.);
#5260=EDGE_CURVE('',#4433,#4434,#2742,.T.);
#5261=EDGE_CURVE('',#4434,#4435,#2743,.T.);
#5262=EDGE_CURVE('',#4436,#4435,#2744,.T.);
#5263=EDGE_CURVE('',#4433,#4436,#2745,.T.);
#5264=EDGE_CURVE('',#4437,#4433,#2746,.T.);
#5265=EDGE_CURVE('',#4438,#4436,#2747,.T.);
#5266=EDGE_CURVE('',#4437,#4438,#2748,.T.);
#5267=EDGE_CURVE('',#4439,#4437,#2749,.T.);
#5268=EDGE_CURVE('',#4440,#4438,#2750,.T.);
#5269=EDGE_CURVE('',#4439,#4440,#2751,.T.);
#5270=EDGE_CURVE('',#4434,#4439,#2752,.T.);
#5271=EDGE_CURVE('',#4435,#4440,#2753,.T.);
#5272=EDGE_CURVE('',#4441,#4442,#2754,.T.);
#5273=EDGE_CURVE('',#4442,#4443,#2755,.T.);
#5274=EDGE_CURVE('',#4444,#4443,#2756,.T.);
#5275=EDGE_CURVE('',#4441,#4444,#2757,.T.);
#5276=EDGE_CURVE('',#4445,#4441,#2758,.T.);
#5277=EDGE_CURVE('',#4446,#4444,#2759,.T.);
#5278=EDGE_CURVE('',#4445,#4446,#2760,.T.);
#5279=EDGE_CURVE('',#4447,#4445,#2761,.T.);
#5280=EDGE_CURVE('',#4448,#4446,#2762,.T.);
#5281=EDGE_CURVE('',#4447,#4448,#2763,.T.);
#5282=EDGE_CURVE('',#4442,#4447,#2764,.T.);
#5283=EDGE_CURVE('',#4443,#4448,#2765,.T.);
#5284=EDGE_CURVE('',#4449,#4449,#3954,.T.);
#5285=EDGE_CURVE('',#4450,#4450,#3955,.T.);
#5286=EDGE_CURVE('',#4450,#4449,#2766,.T.);
#5287=EDGE_CURVE('',#4451,#4451,#3956,.T.);
#5288=EDGE_CURVE('',#4451,#4450,#2767,.T.);
#5289=EDGE_CURVE('',#4452,#4452,#3957,.T.);
#5290=EDGE_CURVE('',#4452,#4451,#2768,.T.);
#5291=EDGE_CURVE('',#4453,#4453,#3958,.T.);
#5292=EDGE_CURVE('',#4454,#4454,#3959,.F.);
#5293=EDGE_CURVE('',#4454,#4453,#2769,.T.);
#5294=EDGE_CURVE('',#4455,#4455,#3960,.F.);
#5295=EDGE_CURVE('',#4455,#4454,#2770,.T.);
#5296=EDGE_CURVE('',#4456,#4456,#3961,.T.);
#5297=EDGE_CURVE('',#4456,#4455,#2771,.T.);
#5298=EDGE_CURVE('',#4457,#4458,#2772,.T.);
#5299=EDGE_CURVE('',#4458,#4459,#2773,.T.);
#5300=EDGE_CURVE('',#4459,#4460,#2774,.T.);
#5301=EDGE_CURVE('',#4457,#4460,#2775,.T.);
#5302=EDGE_CURVE('',#4458,#4461,#2776,.T.);
#5303=EDGE_CURVE('',#4461,#4462,#2777,.T.);
#5304=EDGE_CURVE('',#4462,#4459,#2778,.T.);
#5305=EDGE_CURVE('',#4461,#4463,#2779,.T.);
#5306=EDGE_CURVE('',#4463,#4464,#2780,.T.);
#5307=EDGE_CURVE('',#4464,#4462,#2781,.T.);
#5308=EDGE_CURVE('',#4463,#4465,#2782,.T.);
#5309=EDGE_CURVE('',#4465,#4466,#2783,.T.);
#5310=EDGE_CURVE('',#4466,#4464,#2784,.T.);
#5311=EDGE_CURVE('',#4465,#4467,#2785,.T.);
#5312=EDGE_CURVE('',#4467,#4468,#2786,.T.);
#5313=EDGE_CURVE('',#4468,#4466,#2787,.T.);
#5314=EDGE_CURVE('',#4467,#4457,#2788,.T.);
#5315=EDGE_CURVE('',#4460,#4468,#2789,.T.);
#5316=EDGE_CURVE('',#4469,#4469,#3962,.T.);
#5317=EDGE_CURVE('',#4469,#4470,#2790,.T.);
#5318=EDGE_CURVE('',#4470,#4470,#3963,.T.);
#5319=EDGE_CURVE('',#4471,#4471,#3964,.T.);
#5320=EDGE_CURVE('',#4471,#4472,#2791,.T.);
#5321=EDGE_CURVE('',#4472,#4472,#3965,.T.);
#5322=EDGE_CURVE('',#4473,#4474,#3966,.T.);
#5323=EDGE_CURVE('',#4475,#4476,#2792,.T.);
#5324=EDGE_CURVE('',#4475,#4477,#2793,.T.);
#5325=EDGE_CURVE('',#4476,#4477,#3967,.T.);
#5326=EDGE_CURVE('',#4478,#4479,#2794,.T.);
#5327=EDGE_CURVE('',#4480,#4478,#3968,.T.);
#5328=EDGE_CURVE('',#4480,#4479,#2795,.T.);
#5329=EDGE_CURVE('',#4481,#4482,#2796,.T.);
#5330=EDGE_CURVE('',#4483,#4481,#3969,.T.);
#5331=EDGE_CURVE('',#4483,#4482,#2797,.T.);
#5332=EDGE_CURVE('',#4482,#4475,#2798,.T.);
#5333=EDGE_CURVE('',#4477,#4483,#2799,.T.);
#5334=EDGE_CURVE('',#4484,#4485,#2800,.T.);
#5335=EDGE_CURVE('',#4484,#4486,#2801,.T.);
#5336=EDGE_CURVE('',#4485,#4486,#3970,.T.);
#5337=EDGE_CURVE('',#4479,#4484,#2802,.T.);
#5338=EDGE_CURVE('',#4486,#4480,#2803,.T.);
#5339=EDGE_CURVE('',#4487,#4488,#2804,.T.);
#5340=EDGE_CURVE('',#4488,#4489,#2805,.T.);
#5341=EDGE_CURVE('',#4489,#4490,#2806,.T.);
#5342=EDGE_CURVE('',#4490,#4487,#2807,.T.);
#5343=EDGE_CURVE('',#4491,#4491,#3971,.T.);
#5344=EDGE_CURVE('',#4492,#4492,#3972,.T.);
#5345=EDGE_CURVE('',#4485,#4493,#2808,.T.);
#5346=EDGE_CURVE('',#4493,#4494,#2809,.T.);
#5347=EDGE_CURVE('',#4494,#4481,#2810,.T.);
#5348=EDGE_CURVE('',#4476,#4495,#2811,.T.);
#5349=EDGE_CURVE('',#4495,#4496,#2812,.T.);
#5350=EDGE_CURVE('',#4496,#4478,#2813,.T.);
#5351=EDGE_CURVE('',#4495,#4496,#3973,.T.);
#5352=EDGE_CURVE('',#4493,#4494,#3974,.T.);
#5353=EDGE_CURVE('',#4497,#4498,#2814,.T.);
#5354=EDGE_CURVE('',#4497,#4499,#2815,.T.);
#5355=EDGE_CURVE('',#4499,#4500,#2816,.T.);
#5356=EDGE_CURVE('',#4498,#4500,#2817,.T.);
#5357=EDGE_CURVE('',#4501,#4497,#2818,.T.);
#5358=EDGE_CURVE('',#4501,#4502,#2819,.T.);
#5359=EDGE_CURVE('',#4502,#4499,#2820,.T.);
#5360=EDGE_CURVE('',#4503,#4501,#2821,.T.);
#5361=EDGE_CURVE('',#4503,#4504,#2822,.T.);
#5362=EDGE_CURVE('',#4504,#4502,#2823,.T.);
#5363=EDGE_CURVE('',#4498,#4503,#2824,.T.);
#5364=EDGE_CURVE('',#4500,#4504,#2825,.T.);
#5365=EDGE_CURVE('',#4505,#4505,#3975,.T.);
#5366=EDGE_CURVE('',#4505,#4492,#2826,.T.);
#5367=EDGE_CURVE('',#4506,#4506,#3976,.T.);
#5368=EDGE_CURVE('',#4506,#4491,#2827,.T.);
#5369=EDGE_CURVE('',#4507,#4508,#2828,.T.);
#5370=EDGE_CURVE('',#4508,#4487,#2829,.T.);
#5371=EDGE_CURVE('',#4507,#4490,#2830,.T.);
#5372=EDGE_CURVE('',#4509,#4507,#2831,.T.);
#5373=EDGE_CURVE('',#4509,#4489,#2832,.T.);
#5374=EDGE_CURVE('',#4510,#4509,#2833,.T.);
#5375=EDGE_CURVE('',#4510,#4488,#2834,.T.);
#5376=EDGE_CURVE('',#4508,#4510,#2835,.T.);
#5377=EDGE_CURVE('',#4511,#4511,#3977,.T.);
#5378=EDGE_CURVE('',#4511,#4512,#2836,.T.);
#5379=EDGE_CURVE('',#4512,#4512,#3978,.T.);
#5380=EDGE_CURVE('',#4513,#4513,#3979,.T.);
#5381=EDGE_CURVE('',#4514,#4515,#3980,.T.);
#5382=EDGE_CURVE('',#4516,#4516,#3981,.T.);
#5383=EDGE_CURVE('',#4517,#4518,#457,.T.);
#5384=EDGE_CURVE('',#4519,#4517,#458,.T.);
#5385=EDGE_CURVE('',#4518,#4519,#459,.T.);
#5386=EDGE_CURVE('',#4518,#4520,#2837,.T.);
#5387=EDGE_CURVE('',#4520,#4520,#460,.T.);
#5388=EDGE_CURVE('',#4521,#4521,#461,.T.);
#5389=EDGE_CURVE('',#4521,#4522,#2838,.T.);
#5390=EDGE_CURVE('',#4523,#4522,#462,.T.);
#5391=EDGE_CURVE('',#4524,#4523,#463,.T.);
#5392=EDGE_CURVE('',#4522,#4524,#464,.T.);
#5393=EDGE_CURVE('',#4525,#4525,#3982,.T.);
#5394=EDGE_CURVE('',#4525,#4526,#2839,.T.);
#5395=EDGE_CURVE('',#4526,#4526,#3983,.T.);
#5396=EDGE_CURVE('',#4527,#4528,#465,.T.);
#5397=EDGE_CURVE('',#4528,#4529,#466,.T.);
#5398=EDGE_CURVE('',#4529,#4527,#467,.T.);
#5399=EDGE_CURVE('',#4530,#4531,#468,.T.);
#5400=EDGE_CURVE('',#4531,#4532,#469,.T.);
#5401=EDGE_CURVE('',#4532,#4530,#470,.T.);
#5402=EDGE_CURVE('',#4533,#4534,#471,.T.);
#5403=EDGE_CURVE('',#4534,#4535,#472,.T.);
#5404=EDGE_CURVE('',#4535,#4533,#473,.T.);
#5405=EDGE_CURVE('',#4536,#4537,#474,.T.);
#5406=EDGE_CURVE('',#4537,#4538,#475,.T.);
#5407=EDGE_CURVE('',#4538,#4536,#476,.T.);
#5408=EDGE_CURVE('',#4529,#4539,#2840,.T.);
#5409=EDGE_CURVE('',#4539,#4539,#477,.T.);
#5410=EDGE_CURVE('',#4540,#4540,#478,.T.);
#5411=EDGE_CURVE('',#4540,#4532,#2841,.T.);
#5412=EDGE_CURVE('',#4535,#4541,#2842,.T.);
#5413=EDGE_CURVE('',#4541,#4541,#479,.T.);
#5414=EDGE_CURVE('',#4542,#4542,#480,.T.);
#5415=EDGE_CURVE('',#4542,#4538,#2843,.T.);
#5416=EDGE_CURVE('',#4543,#4543,#3984,.T.);
#5417=EDGE_CURVE('',#4544,#4544,#3985,.T.);
#5418=EDGE_CURVE('',#4545,#4545,#3986,.T.);
#5419=EDGE_CURVE('',#4545,#4544,#2844,.T.);
#5420=EDGE_CURVE('',#4546,#4546,#3987,.T.);
#5421=EDGE_CURVE('',#4546,#4543,#2845,.T.);
#5422=EDGE_CURVE('',#4547,#4547,#3988,.T.);
#5423=EDGE_CURVE('',#4547,#4548,#2846,.T.);
#5424=EDGE_CURVE('',#4548,#4548,#3989,.T.);
#5425=EDGE_CURVE('',#4549,#4549,#3990,.T.);
#5426=EDGE_CURVE('',#4549,#4550,#2847,.T.);
#5427=EDGE_CURVE('',#4550,#4550,#3991,.T.);
#5428=EDGE_CURVE('',#4551,#4552,#2848,.T.);
#5429=EDGE_CURVE('',#4552,#4553,#2849,.T.);
#5430=EDGE_CURVE('',#4553,#4554,#2850,.T.);
#5431=EDGE_CURVE('',#4551,#4554,#2851,.T.);
#5432=EDGE_CURVE('',#4552,#4555,#2852,.T.);
#5433=EDGE_CURVE('',#4555,#4556,#2853,.T.);
#5434=EDGE_CURVE('',#4556,#4553,#2854,.T.);
#5435=EDGE_CURVE('',#4555,#4557,#2855,.T.);
#5436=EDGE_CURVE('',#4557,#4558,#2856,.T.);
#5437=EDGE_CURVE('',#4558,#4556,#2857,.T.);
#5438=EDGE_CURVE('',#4557,#4559,#2858,.T.);
#5439=EDGE_CURVE('',#4559,#4560,#2859,.T.);
#5440=EDGE_CURVE('',#4560,#4558,#2860,.T.);
#5441=EDGE_CURVE('',#4559,#4561,#2861,.T.);
#5442=EDGE_CURVE('',#4561,#4562,#2862,.T.);
#5443=EDGE_CURVE('',#4562,#4560,#2863,.T.);
#5444=EDGE_CURVE('',#4561,#4551,#2864,.T.);
#5445=EDGE_CURVE('',#4554,#4562,#2865,.T.);
#5446=EDGE_CURVE('',#4563,#4563,#3992,.T.);
#5447=EDGE_CURVE('',#4564,#4564,#3993,.T.);
#5448=EDGE_CURVE('',#4565,#4565,#3994,.T.);
#5449=EDGE_CURVE('',#4565,#4564,#2866,.T.);
#5450=EDGE_CURVE('',#4566,#4566,#3995,.T.);
#5451=EDGE_CURVE('',#4566,#4565,#2867,.T.);
#5452=EDGE_CURVE('',#4567,#4567,#3996,.T.);
#5453=EDGE_CURVE('',#4567,#4566,#2868,.T.);
#5454=EDGE_CURVE('',#4568,#4568,#3997,.T.);
#5455=EDGE_CURVE('',#4569,#4569,#3998,.F.);
#5456=EDGE_CURVE('',#4569,#4568,#2869,.T.);
#5457=EDGE_CURVE('',#4563,#4569,#2870,.T.);
#5458=EDGE_CURVE('',#4570,#4571,#2871,.T.);
#5459=EDGE_CURVE('',#4571,#4570,#3999,.T.);
#5460=EDGE_CURVE('',#4572,#4570,#2872,.T.);
#5461=EDGE_CURVE('',#4573,#4572,#4000,.T.);
#5462=EDGE_CURVE('',#4571,#4573,#2873,.T.);
#5463=EDGE_CURVE('',#4574,#4575,#2874,.T.);
#5464=EDGE_CURVE('',#4574,#4576,#4001,.T.);
#5465=EDGE_CURVE('',#4577,#4576,#2875,.T.);
#5466=EDGE_CURVE('',#4575,#4577,#4002,.T.);
#5467=EDGE_CURVE('',#4576,#4574,#2876,.T.);
#5468=EDGE_CURVE('',#4572,#4578,#2877,.T.);
#5469=EDGE_CURVE('',#4579,#4578,#2878,.T.);
#5470=EDGE_CURVE('',#4579,#4580,#2879,.T.);
#5471=EDGE_CURVE('',#4581,#4580,#2880,.T.);
#5472=EDGE_CURVE('',#4581,#4573,#2881,.T.);
#5473=EDGE_CURVE('',#4582,#4582,#4003,.T.);
#5474=EDGE_CURVE('',#4583,#4581,#2882,.T.);
#5475=EDGE_CURVE('',#4583,#4584,#2883,.T.);
#5476=EDGE_CURVE('',#4578,#4584,#2884,.T.);
#5477=EDGE_CURVE('',#4585,#4585,#4004,.T.);
#5478=EDGE_CURVE('',#4586,#4587,#2885,.T.);
#5479=EDGE_CURVE('',#4588,#4587,#2886,.T.);
#5480=EDGE_CURVE('',#4575,#4588,#2887,.T.);
#5481=EDGE_CURVE('',#4589,#4577,#2888,.T.);
#5482=EDGE_CURVE('',#4586,#4589,#2889,.T.);
#5483=EDGE_CURVE('',#4590,#4590,#4005,.T.);
#5484=EDGE_CURVE('',#4591,#4591,#4006,.T.);
#5485=EDGE_CURVE('',#4591,#4592,#2890,.T.);
#5486=EDGE_CURVE('',#4592,#4592,#4007,.T.);
#5487=EDGE_CURVE('',#4585,#4593,#2891,.T.);
#5488=EDGE_CURVE('',#4593,#4593,#4008,.T.);
#5489=EDGE_CURVE('',#4594,#4594,#4009,.T.);
#5490=EDGE_CURVE('',#4594,#4582,#2892,.T.);
#5491=EDGE_CURVE('',#4595,#4595,#4010,.T.);
#5492=EDGE_CURVE('',#4595,#4590,#2893,.T.);
#5493=EDGE_CURVE('',#4596,#4596,#4011,.T.);
#5494=EDGE_CURVE('',#4596,#4597,#2894,.T.);
#5495=EDGE_CURVE('',#4597,#4597,#4012,.T.);
#5496=EDGE_CURVE('',#4580,#4598,#2895,.T.);
#5497=EDGE_CURVE('',#4598,#4599,#2896,.T.);
#5498=EDGE_CURVE('',#4599,#4586,#2897,.T.);
#5499=EDGE_CURVE('',#4589,#4600,#2898,.T.);
#5500=EDGE_CURVE('',#4600,#4601,#2899,.T.);
#5501=EDGE_CURVE('',#4601,#4602,#2900,.T.);
#5502=EDGE_CURVE('',#4602,#4603,#2901,.T.);
#5503=EDGE_CURVE('',#4603,#4604,#2902,.T.);
#5504=EDGE_CURVE('',#4604,#4583,#2903,.T.);
#5505=EDGE_CURVE('',#4605,#4579,#2904,.T.);
#5506=EDGE_CURVE('',#4598,#4605,#2905,.T.);
#5507=EDGE_CURVE('',#4606,#4605,#2906,.T.);
#5508=EDGE_CURVE('',#4599,#4606,#2907,.T.);
#5509=EDGE_CURVE('',#4587,#4606,#2908,.T.);
#5510=EDGE_CURVE('',#4607,#4588,#2909,.T.);
#5511=EDGE_CURVE('',#4600,#4607,#2910,.T.);
#5512=EDGE_CURVE('',#4608,#4607,#2911,.T.);
#5513=EDGE_CURVE('',#4601,#4608,#2912,.T.);
#5514=EDGE_CURVE('',#4609,#4608,#2913,.T.);
#5515=EDGE_CURVE('',#4602,#4609,#2914,.T.);
#5516=EDGE_CURVE('',#4610,#4609,#2915,.T.);
#5517=EDGE_CURVE('',#4603,#4610,#2916,.T.);
#5518=EDGE_CURVE('',#4611,#4610,#2917,.T.);
#5519=EDGE_CURVE('',#4604,#4611,#2918,.T.);
#5520=EDGE_CURVE('',#4584,#4611,#2919,.T.);
#5521=EDGE_CURVE('',#4612,#4612,#4013,.T.);
#5522=EDGE_CURVE('',#4612,#4613,#2920,.T.);
#5523=EDGE_CURVE('',#4613,#4613,#4014,.T.);
#5524=EDGE_CURVE('',#4613,#4614,#2921,.T.);
#5525=EDGE_CURVE('',#4614,#4614,#4015,.T.);
#5526=EDGE_CURVE('',#4615,#4615,#4016,.T.);
#5527=EDGE_CURVE('',#4615,#4616,#2922,.T.);
#5528=EDGE_CURVE('',#4616,#4616,#4017,.T.);
#5529=EDGE_CURVE('',#4617,#4618,#2923,.T.);
#5530=EDGE_CURVE('',#4618,#4619,#2924,.T.);
#5531=EDGE_CURVE('',#4619,#4620,#2925,.T.);
#5532=EDGE_CURVE('',#4617,#4620,#2926,.T.);
#5533=EDGE_CURVE('',#4618,#4621,#2927,.T.);
#5534=EDGE_CURVE('',#4621,#4622,#2928,.T.);
#5535=EDGE_CURVE('',#4622,#4619,#2929,.T.);
#5536=EDGE_CURVE('',#4621,#4623,#2930,.T.);
#5537=EDGE_CURVE('',#4623,#4624,#2931,.T.);
#5538=EDGE_CURVE('',#4624,#4622,#2932,.T.);
#5539=EDGE_CURVE('',#4623,#4625,#2933,.T.);
#5540=EDGE_CURVE('',#4625,#4626,#2934,.T.);
#5541=EDGE_CURVE('',#4626,#4624,#2935,.T.);
#5542=EDGE_CURVE('',#4625,#4627,#2936,.T.);
#5543=EDGE_CURVE('',#4627,#4628,#2937,.T.);
#5544=EDGE_CURVE('',#4628,#4626,#2938,.T.);
#5545=EDGE_CURVE('',#4627,#4617,#2939,.T.);
#5546=EDGE_CURVE('',#4620,#4628,#2940,.T.);
#5547=EDGE_CURVE('',#4629,#4629,#4018,.T.);
#5548=EDGE_CURVE('',#4630,#4630,#4019,.T.);
#5549=EDGE_CURVE('',#4631,#4631,#4020,.T.);
#5550=EDGE_CURVE('',#4631,#4630,#2941,.T.);
#5551=EDGE_CURVE('',#4632,#4632,#4021,.T.);
#5552=EDGE_CURVE('',#4632,#4631,#2942,.T.);
#5553=EDGE_CURVE('',#4633,#4633,#4022,.T.);
#5554=EDGE_CURVE('',#4633,#4632,#2943,.T.);
#5555=EDGE_CURVE('',#4634,#4634,#4023,.T.);
#5556=EDGE_CURVE('',#4635,#4635,#4024,.F.);
#5557=EDGE_CURVE('',#4635,#4634,#2944,.T.);
#5558=EDGE_CURVE('',#4629,#4635,#2945,.T.);
#5559=EDGE_CURVE('',#4636,#4636,#4025,.T.);
#5560=EDGE_CURVE('',#4637,#4637,#4026,.T.);
#5561=EDGE_CURVE('',#4637,#4636,#2946,.T.);
#5562=EDGE_CURVE('',#4638,#4638,#4027,.T.);
#5563=EDGE_CURVE('',#4638,#4637,#2947,.T.);
#5564=EDGE_CURVE('',#4639,#4639,#4028,.T.);
#5565=EDGE_CURVE('',#4639,#4638,#2948,.T.);
#5566=EDGE_CURVE('',#4640,#4640,#4029,.T.);
#5567=EDGE_CURVE('',#4641,#4641,#4030,.F.);
#5568=EDGE_CURVE('',#4641,#4640,#2949,.T.);
#5569=EDGE_CURVE('',#4642,#4642,#4031,.F.);
#5570=EDGE_CURVE('',#4642,#4641,#2950,.T.);
#5571=EDGE_CURVE('',#4643,#4643,#4032,.T.);
#5572=EDGE_CURVE('',#4643,#4642,#2951,.T.);
#5573=EDGE_CURVE('',#4644,#4645,#2952,.T.);
#5574=EDGE_CURVE('',#4645,#4646,#2953,.T.);
#5575=EDGE_CURVE('',#4646,#4647,#2954,.T.);
#5576=EDGE_CURVE('',#4644,#4647,#2955,.T.);
#5577=EDGE_CURVE('',#4645,#4648,#2956,.T.);
#5578=EDGE_CURVE('',#4648,#4649,#2957,.T.);
#5579=EDGE_CURVE('',#4649,#4646,#2958,.T.);
#5580=EDGE_CURVE('',#4648,#4650,#2959,.T.);
#5581=EDGE_CURVE('',#4650,#4651,#2960,.T.);
#5582=EDGE_CURVE('',#4651,#4649,#2961,.T.);
#5583=EDGE_CURVE('',#4650,#4652,#2962,.T.);
#5584=EDGE_CURVE('',#4652,#4653,#2963,.T.);
#5585=EDGE_CURVE('',#4653,#4651,#2964,.T.);
#5586=EDGE_CURVE('',#4652,#4654,#2965,.T.);
#5587=EDGE_CURVE('',#4654,#4655,#2966,.T.);
#5588=EDGE_CURVE('',#4655,#4653,#2967,.T.);
#5589=EDGE_CURVE('',#4654,#4644,#2968,.T.);
#5590=EDGE_CURVE('',#4647,#4655,#2969,.T.);
#5591=EDGE_CURVE('',#4656,#4656,#4033,.T.);
#5592=EDGE_CURVE('',#4657,#4657,#4034,.T.);
#5593=EDGE_CURVE('',#4657,#4658,#2970,.T.);
#5594=EDGE_CURVE('',#4658,#4658,#4035,.T.);
#5595=EDGE_CURVE('',#4656,#4657,#2971,.T.);
#5596=EDGE_CURVE('',#4659,#4660,#2972,.T.);
#5597=EDGE_CURVE('',#4661,#4659,#2973,.T.);
#5598=EDGE_CURVE('',#4662,#4661,#2974,.T.);
#5599=EDGE_CURVE('',#4662,#4660,#2975,.T.);
#5600=EDGE_CURVE('',#4660,#4663,#4036,.T.);
#5601=EDGE_CURVE('',#4664,#4662,#2976,.T.);
#5602=EDGE_CURVE('',#4663,#4664,#2977,.T.);
#5603=EDGE_CURVE('',#4663,#4665,#2978,.T.);
#5604=EDGE_CURVE('',#4664,#4666,#2979,.T.);
#5605=EDGE_CURVE('',#4665,#4666,#2980,.T.);
#5606=EDGE_CURVE('',#4666,#4661,#2981,.T.);
#5607=EDGE_CURVE('',#4667,#4665,#4037,.T.);
#5608=EDGE_CURVE('',#4667,#4668,#2982,.T.);
#5609=EDGE_CURVE('',#4668,#4668,#4038,.T.);
#5610=EDGE_CURVE('',#4659,#4667,#4039,.T.);
#5611=EDGE_CURVE('',#4669,#4670,#2983,.T.);
#5612=EDGE_CURVE('',#4669,#4670,#4040,.T.);
#5613=EDGE_CURVE('',#4671,#4669,#481,.T.);
#5614=EDGE_CURVE('',#4672,#4671,#4041,.T.);
#5615=EDGE_CURVE('',#4672,#4673,#2984,.T.);
#5616=EDGE_CURVE('',#4674,#4673,#482,.T.);
#5617=EDGE_CURVE('',#4673,#4674,#483,.T.);
#5618=EDGE_CURVE('',#4675,#4672,#4042,.T.);
#5619=EDGE_CURVE('',#4670,#4675,#484,.T.);
#5620=EDGE_CURVE('',#4675,#4671,#2985,.T.);
#5621=EDGE_CURVE('',#4676,#4676,#4043,.T.);
#5622=EDGE_CURVE('',#4676,#4677,#2986,.T.);
#5623=EDGE_CURVE('',#4677,#4677,#4044,.T.);
#5624=EDGE_CURVE('',#4678,#4678,#4045,.T.);
#5625=EDGE_CURVE('',#4678,#4679,#2987,.T.);
#5626=EDGE_CURVE('',#4679,#4679,#4046,.T.);
#5627=EDGE_CURVE('',#4680,#4681,#2988,.T.);
#5628=EDGE_CURVE('',#4680,#4681,#4047,.T.);
#5629=EDGE_CURVE('',#4682,#4680,#485,.T.);
#5630=EDGE_CURVE('',#4683,#4682,#4048,.T.);
#5631=EDGE_CURVE('',#4683,#4684,#2989,.T.);
#5632=EDGE_CURVE('',#4685,#4684,#486,.T.);
#5633=EDGE_CURVE('',#4684,#4685,#487,.T.);
#5634=EDGE_CURVE('',#4686,#4683,#4049,.T.);
#5635=EDGE_CURVE('',#4681,#4686,#488,.T.);
#5636=EDGE_CURVE('',#4686,#4682,#2990,.T.);
#5637=EDGE_CURVE('',#4687,#4687,#4050,.T.);
#5638=EDGE_CURVE('',#4687,#4688,#2991,.T.);
#5639=EDGE_CURVE('',#4688,#4688,#4051,.T.);
#5640=EDGE_CURVE('',#4689,#4689,#4052,.T.);
#5641=EDGE_CURVE('',#4689,#4690,#2992,.T.);
#5642=EDGE_CURVE('',#4690,#4690,#4053,.T.);
#5643=EDGE_CURVE('',#4691,#4691,#4054,.T.);
#5644=EDGE_CURVE('',#4691,#4692,#2993,.T.);
#5645=EDGE_CURVE('',#4692,#4692,#4055,.T.);
#5646=EDGE_CURVE('',#4693,#4693,#4056,.T.);
#5647=EDGE_CURVE('',#4693,#4694,#2994,.T.);
#5648=EDGE_CURVE('',#4694,#4694,#4057,.T.);
#5649=EDGE_CURVE('',#4695,#4696,#2995,.T.);
#5650=EDGE_CURVE('',#4697,#4695,#4058,.T.);
#5651=EDGE_CURVE('',#4698,#4697,#2996,.T.);
#5652=EDGE_CURVE('',#4696,#4698,#4059,.T.);
#5653=EDGE_CURVE('',#4698,#4696,#4060,.T.);
#5654=EDGE_CURVE('',#4699,#4700,#2997,.T.);
#5655=EDGE_CURVE('',#4700,#4701,#2998,.T.);
#5656=EDGE_CURVE('',#4701,#4702,#2999,.T.);
#5657=EDGE_CURVE('',#4702,#4699,#4061,.T.);
#5658=EDGE_CURVE('',#4703,#4703,#4062,.T.);
#5659=EDGE_CURVE('',#4703,#4704,#3000,.T.);
#5660=EDGE_CURVE('',#4704,#4704,#4063,.T.);
#5661=EDGE_CURVE('',#4705,#4706,#3001,.T.);
#5662=EDGE_CURVE('',#4705,#4706,#4064,.T.);
#5663=EDGE_CURVE('',#4707,#4705,#489,.T.);
#5664=EDGE_CURVE('',#4708,#4707,#4065,.T.);
#5665=EDGE_CURVE('',#4709,#4708,#490,.T.);
#5666=EDGE_CURVE('',#4710,#4709,#3002,.T.);
#5667=EDGE_CURVE('',#4711,#4710,#491,.T.);
#5668=EDGE_CURVE('',#4712,#4711,#3003,.T.);
#5669=EDGE_CURVE('',#4706,#4712,#492,.T.);
#5670=EDGE_CURVE('',#4708,#4707,#3004,.T.);
#5671=EDGE_CURVE('',#4712,#4713,#4066,.T.);
#5672=EDGE_CURVE('',#4713,#4699,#3005,.T.);
#5673=EDGE_CURVE('',#4702,#4714,#3006,.T.);
#5674=EDGE_CURVE('',#4714,#4709,#4067,.T.);
#5675=EDGE_CURVE('',#4715,#4713,#3007,.T.);
#5676=EDGE_CURVE('',#4715,#4700,#3008,.T.);
#5677=EDGE_CURVE('',#4716,#4715,#3009,.T.);
#5678=EDGE_CURVE('',#4716,#4701,#3010,.T.);
#5679=EDGE_CURVE('',#4714,#4716,#3011,.T.);
#5680=EDGE_CURVE('',#4717,#4717,#4068,.T.);
#5681=EDGE_CURVE('',#4697,#4695,#4069,.T.);
#5682=EDGE_CURVE('',#4718,#4718,#4070,.T.);
#5683=EDGE_CURVE('',#4719,#4719,#4071,.T.);
#5684=EDGE_CURVE('',#4717,#4718,#3012,.T.);
#5685=EDGE_CURVE('',#4719,#4720,#3013,.T.);
#5686=EDGE_CURVE('',#4720,#4711,#4072,.T.);
#5687=EDGE_CURVE('',#4710,#4720,#4073,.T.);
#5688=EDGE_CURVE('',#4721,#4721,#4074,.T.);
#5689=EDGE_CURVE('',#4721,#4722,#3014,.T.);
#5690=EDGE_CURVE('',#4722,#4722,#4075,.T.);
#5691=EDGE_CURVE('',#4723,#4723,#4076,.T.);
#5692=EDGE_CURVE('',#4724,#4724,#4077,.T.);
#5693=EDGE_CURVE('',#4725,#4725,#4078,.T.);
#5694=EDGE_CURVE('',#4725,#4723,#3015,.T.);
#5695=EDGE_CURVE('',#4724,#4726,#3016,.T.);
#5696=EDGE_CURVE('',#4726,#4726,#4079,.T.);
#5697=EDGE_CURVE('',#4727,#4727,#4080,.T.);
#5698=EDGE_CURVE('',#4727,#4728,#3017,.T.);
#5699=EDGE_CURVE('',#4728,#4728,#4081,.T.);
#5700=EDGE_CURVE('',#4729,#4729,#4082,.T.);
#5701=EDGE_CURVE('',#4729,#4730,#3018,.T.);
#5702=EDGE_CURVE('',#4730,#4730,#4083,.T.);
#5703=EDGE_CURVE('',#4731,#4731,#4084,.T.);
#5704=EDGE_CURVE('',#4731,#4732,#3019,.T.);
#5705=EDGE_CURVE('',#4732,#4732,#4085,.T.);
#5706=EDGE_CURVE('',#4733,#4733,#4086,.T.);
#5707=EDGE_CURVE('',#4733,#4734,#3020,.T.);
#5708=EDGE_CURVE('',#4734,#4734,#4087,.T.);
#5709=EDGE_CURVE('',#4735,#4735,#4088,.T.);
#5710=EDGE_CURVE('',#4735,#4736,#3021,.T.);
#5711=EDGE_CURVE('',#4736,#4736,#4089,.T.);
#5712=EDGE_CURVE('',#4737,#4737,#4090,.T.);
#5713=EDGE_CURVE('',#4737,#4738,#3022,.T.);
#5714=EDGE_CURVE('',#4738,#4738,#4091,.T.);
#5715=EDGE_CURVE('',#4739,#4740,#3023,.T.);
#5716=EDGE_CURVE('',#4741,#4739,#3024,.T.);
#5717=EDGE_CURVE('',#4742,#4741,#3025,.T.);
#5718=EDGE_CURVE('',#4743,#4742,#3026,.T.);
#5719=EDGE_CURVE('',#4744,#4743,#3027,.T.);
#5720=EDGE_CURVE('',#4745,#4744,#3028,.T.);
#5721=EDGE_CURVE('',#4746,#4745,#3029,.T.);
#5722=EDGE_CURVE('',#4740,#4746,#3030,.T.);
#5723=EDGE_CURVE('',#4743,#4747,#3031,.T.);
#5724=EDGE_CURVE('',#4747,#4748,#3032,.T.);
#5725=EDGE_CURVE('',#4748,#4744,#3033,.T.);
#5726=EDGE_CURVE('',#4749,#4742,#3034,.T.);
#5727=EDGE_CURVE('',#4749,#4747,#3035,.T.);
#5728=EDGE_CURVE('',#4741,#4750,#3036,.T.);
#5729=EDGE_CURVE('',#4750,#4749,#3037,.T.);
#5730=EDGE_CURVE('',#4751,#4739,#3038,.T.);
#5731=EDGE_CURVE('',#4751,#4750,#3039,.T.);
#5732=EDGE_CURVE('',#4752,#4753,#3040,.T.);
#5733=EDGE_CURVE('',#4748,#4752,#3041,.T.);
#5734=EDGE_CURVE('',#4754,#4751,#3042,.T.);
#5735=EDGE_CURVE('',#4753,#4754,#3043,.T.);
#5736=EDGE_CURVE('',#4745,#4752,#3044,.T.);
#5737=EDGE_CURVE('',#4740,#4754,#3045,.T.);
#5738=EDGE_CURVE('',#4753,#4746,#3046,.T.);
#5739=EDGE_CURVE('',#4755,#4756,#3047,.T.);
#5740=EDGE_CURVE('',#4755,#4757,#3048,.T.);
#5741=EDGE_CURVE('',#4757,#4758,#3049,.T.);
#5742=EDGE_CURVE('',#4756,#4758,#3050,.T.);
#5743=EDGE_CURVE('',#4759,#4755,#3051,.T.);
#5744=EDGE_CURVE('',#4759,#4760,#3052,.T.);
#5745=EDGE_CURVE('',#4760,#4757,#3053,.T.);
#5746=EDGE_CURVE('',#4761,#4759,#3054,.T.);
#5747=EDGE_CURVE('',#4761,#4762,#3055,.T.);
#5748=EDGE_CURVE('',#4762,#4760,#3056,.T.);
#5749=EDGE_CURVE('',#4763,#4761,#3057,.T.);
#5750=EDGE_CURVE('',#4763,#4764,#3058,.T.);
#5751=EDGE_CURVE('',#4764,#4762,#3059,.T.);
#5752=EDGE_CURVE('',#4765,#4763,#3060,.T.);
#5753=EDGE_CURVE('',#4765,#4766,#3061,.T.);
#5754=EDGE_CURVE('',#4766,#4764,#3062,.T.);
#5755=EDGE_CURVE('',#4756,#4765,#3063,.T.);
#5756=EDGE_CURVE('',#4758,#4766,#3064,.T.);
#5757=EDGE_CURVE('',#4767,#4767,#4092,.T.);
#5758=EDGE_CURVE('',#4768,#4768,#4093,.T.);
#5759=EDGE_CURVE('',#4768,#4767,#3065,.T.);
#5760=EDGE_CURVE('',#4769,#4769,#4094,.F.);
#5761=EDGE_CURVE('',#4769,#4768,#3066,.T.);
#5762=EDGE_CURVE('',#4770,#4770,#4095,.T.);
#5763=EDGE_CURVE('',#4770,#4769,#3067,.T.);
#5764=EDGE_CURVE('',#4771,#4771,#4096,.T.);
#5765=EDGE_CURVE('',#4771,#4772,#3068,.T.);
#5766=EDGE_CURVE('',#4772,#4772,#4097,.T.);
#5767=EDGE_CURVE('',#4773,#4773,#4098,.T.);
#5768=EDGE_CURVE('',#4773,#4774,#3069,.T.);
#5769=EDGE_CURVE('',#4774,#4774,#4099,.T.);
#5770=EDGE_CURVE('',#4775,#4776,#3070,.T.);
#5771=EDGE_CURVE('',#4775,#4777,#4100,.T.);
#5772=EDGE_CURVE('',#4778,#4777,#3071,.T.);
#5773=EDGE_CURVE('',#4776,#4778,#4101,.T.);
#5774=EDGE_CURVE('',#4778,#4779,#3072,.T.);
#5775=EDGE_CURVE('',#4779,#4780,#4102,.T.);
#5776=EDGE_CURVE('',#4780,#4776,#3073,.T.);
#5777=EDGE_CURVE('',#4781,#4777,#3074,.T.);
#5778=EDGE_CURVE('',#4781,#4779,#3075,.T.);
#5779=EDGE_CURVE('',#4780,#4782,#3076,.T.);
#5780=EDGE_CURVE('',#4781,#4782,#4103,.T.);
#5781=EDGE_CURVE('',#4775,#4782,#3077,.T.);
#5782=EDGE_CURVE('',#4783,#4783,#4104,.T.);
#5783=EDGE_CURVE('',#4783,#4784,#3078,.T.);
#5784=EDGE_CURVE('',#4784,#4784,#4105,.T.);
#5785=EDGE_CURVE('',#4785,#4785,#4106,.T.);
#5786=EDGE_CURVE('',#4785,#4786,#3079,.T.);
#5787=EDGE_CURVE('',#4786,#4786,#4107,.T.);
#5788=EDGE_CURVE('',#4787,#4787,#4108,.T.);
#5789=EDGE_CURVE('',#4787,#4788,#3080,.T.);
#5790=EDGE_CURVE('',#4788,#4788,#4109,.T.);
#5791=EDGE_CURVE('',#4789,#4789,#4110,.T.);
#5792=EDGE_CURVE('',#4789,#4790,#3081,.T.);
#5793=EDGE_CURVE('',#4790,#4790,#4111,.T.);
#5794=EDGE_CURVE('',#4791,#4791,#4112,.T.);
#5795=EDGE_CURVE('',#4791,#4792,#3082,.T.);
#5796=EDGE_CURVE('',#4792,#4792,#4113,.T.);
#5797=EDGE_CURVE('',#4793,#4793,#4114,.T.);
#5798=EDGE_CURVE('',#4793,#4794,#3083,.T.);
#5799=EDGE_CURVE('',#4794,#4794,#4115,.T.);
#5800=EDGE_CURVE('',#4795,#4795,#4116,.T.);
#5801=EDGE_CURVE('',#4795,#4796,#3084,.T.);
#5802=EDGE_CURVE('',#4796,#4796,#4117,.T.);
#5803=EDGE_CURVE('',#4797,#4797,#4118,.T.);
#5804=EDGE_CURVE('',#4797,#4798,#3085,.T.);
#5805=EDGE_CURVE('',#4798,#4798,#4119,.T.);
#5806=EDGE_CURVE('',#4799,#4800,#4120,.T.);
#5807=EDGE_CURVE('',#4800,#4799,#4121,.T.);
#5808=EDGE_CURVE('',#4800,#4801,#4122,.T.);
#5809=EDGE_CURVE('',#4802,#4801,#4123,.T.);
#5810=EDGE_CURVE('',#4801,#4802,#4124,.T.);
#5811=EDGE_CURVE('',#4802,#4803,#3086,.T.);
#5812=EDGE_CURVE('',#4803,#4803,#4125,.T.);
#5813=EDGE_CURVE('',#4804,#4804,#4126,.T.);
#5814=EDGE_CURVE('',#4804,#4805,#3087,.T.);
#5815=EDGE_CURVE('',#4805,#4805,#4127,.T.);
#5816=EDGE_CURVE('',#4805,#4806,#3088,.T.);
#5817=EDGE_CURVE('',#4806,#4806,#4128,.T.);
#5818=EDGE_CURVE('',#4807,#4807,#4129,.T.);
#5819=EDGE_CURVE('',#4807,#4799,#3089,.T.);
#5820=EDGE_CURVE('',#4808,#4808,#4130,.T.);
#5821=EDGE_CURVE('',#4808,#4804,#3090,.T.);
#5822=EDGE_CURVE('',#4809,#4810,#4131,.T.);
#5823=EDGE_CURVE('',#4810,#4809,#4132,.T.);
#5824=EDGE_CURVE('',#4810,#4811,#4133,.T.);
#5825=EDGE_CURVE('',#4812,#4811,#4134,.T.);
#5826=EDGE_CURVE('',#4811,#4812,#4135,.T.);
#5827=EDGE_CURVE('',#4813,#4813,#4136,.T.);
#5828=EDGE_CURVE('',#4813,#4812,#3091,.T.);
#5829=EDGE_CURVE('',#4814,#4814,#4137,.T.);
#5830=EDGE_CURVE('',#4815,#4815,#4138,.T.);
#5831=EDGE_CURVE('',#4816,#4816,#4139,.T.);
#5832=EDGE_CURVE('',#4816,#4814,#3092,.T.);
#5833=EDGE_CURVE('',#4817,#4817,#4140,.T.);
#5834=EDGE_CURVE('',#4817,#4816,#3093,.T.);
#5835=EDGE_CURVE('',#4818,#4818,#4141,.T.);
#5836=EDGE_CURVE('',#4818,#4817,#3094,.T.);
#5837=EDGE_CURVE('',#4809,#4815,#3095,.T.);
#5838=EDGE_CURVE('',#4819,#4820,#4142,.T.);
#5839=EDGE_CURVE('',#4821,#4822,#4143,.T.);
#5840=EDGE_CURVE('',#4823,#4824,#4144,.T.);
#5841=EDGE_CURVE('',#4825,#4826,#4145,.T.);
#5842=EDGE_CURVE('',#4827,#4828,#4146,.T.);
#5843=EDGE_CURVE('',#4829,#4830,#4147,.T.);
#5844=EDGE_CURVE('',#4831,#4832,#4148,.T.);
#5845=EDGE_CURVE('',#4833,#4834,#4149,.T.);
#5846=EDGE_CURVE('',#4835,#4836,#493,.T.);
#5847=EDGE_CURVE('',#4837,#4835,#4150,.T.);
#5848=EDGE_CURVE('',#4838,#4837,#494,.T.);
#5849=EDGE_CURVE('',#4836,#4838,#4151,.T.);
#5850=EDGE_CURVE('',#4839,#4837,#4152,.T.);
#5851=EDGE_CURVE('',#4839,#4840,#495,.T.);
#5852=EDGE_CURVE('',#4841,#4840,#4153,.T.);
#5853=EDGE_CURVE('',#4841,#4842,#496,.T.);
#5854=EDGE_CURVE('',#4843,#4842,#4154,.T.);
#5855=EDGE_CURVE('',#4843,#4844,#497,.T.);
#5856=EDGE_CURVE('',#4844,#4845,#3096,.T.);
#5857=EDGE_CURVE('',#4845,#4845,#4155,.T.);
#5858=EDGE_CURVE('',#4844,#4846,#498,.T.);
#5859=EDGE_CURVE('',#4847,#4846,#4156,.T.);
#5860=EDGE_CURVE('',#4847,#4848,#499,.T.);
#5861=EDGE_CURVE('',#4849,#4848,#4157,.T.);
#5862=EDGE_CURVE('',#4849,#4850,#500,.T.);
#5863=EDGE_CURVE('',#4851,#4850,#4158,.T.);
#5864=EDGE_CURVE('',#4851,#4852,#501,.T.);
#5865=EDGE_CURVE('',#4853,#4852,#4159,.T.);
#5866=EDGE_CURVE('',#4853,#4854,#502,.T.);
#5867=EDGE_CURVE('',#4838,#4854,#4160,.T.);
#5868=EDGE_CURVE('',#4835,#4855,#4161,.T.);
#5869=EDGE_CURVE('',#4855,#4839,#4162,.T.);
#5870=EDGE_CURVE('',#4856,#4855,#503,.T.);
#5871=EDGE_CURVE('',#4840,#4856,#4163,.T.);
#5872=EDGE_CURVE('',#4856,#4857,#4164,.T.);
#5873=EDGE_CURVE('',#4857,#4841,#4165,.T.);
#5874=EDGE_CURVE('',#4858,#4857,#504,.T.);
#5875=EDGE_CURVE('',#4842,#4858,#4166,.T.);
#5876=EDGE_CURVE('',#4858,#4859,#4167,.T.);
#5877=EDGE_CURVE('',#4859,#4843,#4168,.T.);
#5878=EDGE_CURVE('',#4860,#4861,#505,.T.);
#5879=EDGE_CURVE('',#4846,#4860,#4169,.T.);
#5880=EDGE_CURVE('',#4861,#4859,#506,.T.);
#5881=EDGE_CURVE('',#4860,#4862,#4170,.T.);
#5882=EDGE_CURVE('',#4862,#4847,#4171,.T.);
#5883=EDGE_CURVE('',#4863,#4862,#507,.T.);
#5884=EDGE_CURVE('',#4848,#4863,#4172,.T.);
#5885=EDGE_CURVE('',#4863,#4864,#4173,.T.);
#5886=EDGE_CURVE('',#4864,#4849,#4174,.T.);
#5887=EDGE_CURVE('',#4865,#4864,#508,.T.);
#5888=EDGE_CURVE('',#4850,#4865,#4175,.T.);
#5889=EDGE_CURVE('',#4865,#4866,#4176,.T.);
#5890=EDGE_CURVE('',#4866,#4851,#4177,.T.);
#5891=EDGE_CURVE('',#4867,#4866,#509,.T.);
#5892=EDGE_CURVE('',#4852,#4867,#4178,.T.);
#5893=EDGE_CURVE('',#4868,#4868,#4179,.T.);
#5894=EDGE_CURVE('',#4868,#4861,#3097,.T.);
#5895=EDGE_CURVE('',#4869,#4836,#4180,.T.);
#5896=EDGE_CURVE('',#4869,#4870,#510,.T.);
#5897=EDGE_CURVE('',#4867,#4870,#4181,.T.);
#5898=EDGE_CURVE('',#4854,#4869,#4182,.T.);
#5899=EDGE_CURVE('',#4870,#4853,#4183,.T.);
#5900=EDGE_CURVE('',#4871,#4871,#4184,.T.);
#5901=EDGE_CURVE('',#4872,#4872,#4185,.T.);
#5902=EDGE_CURVE('',#4873,#4873,#4186,.T.);
#5903=EDGE_CURVE('',#4873,#4871,#3098,.T.);
#5904=EDGE_CURVE('',#4874,#4874,#4187,.T.);
#5905=EDGE_CURVE('',#4874,#4872,#3099,.T.);
#5906=EDGE_CURVE('',#4875,#4875,#4188,.T.);
#5907=EDGE_CURVE('',#4876,#4876,#4189,.T.);
#5908=EDGE_CURVE('',#4877,#4877,#4190,.T.);
#5909=EDGE_CURVE('',#4877,#4875,#3100,.T.);
#5910=EDGE_CURVE('',#4878,#4878,#4191,.T.);
#5911=EDGE_CURVE('',#4878,#4876,#3101,.T.);
#5912=EDGE_CURVE('',#4879,#4879,#4192,.T.);
#5913=EDGE_CURVE('',#4879,#4880,#3102,.T.);
#5914=EDGE_CURVE('',#4880,#4880,#4193,.T.);
#5915=EDGE_CURVE('',#4881,#4882,#3103,.T.);
#5916=EDGE_CURVE('',#4881,#4883,#3104,.T.);
#5917=EDGE_CURVE('',#4883,#4884,#3105,.T.);
#5918=EDGE_CURVE('',#4884,#4882,#3106,.T.);
#5919=EDGE_CURVE('',#4885,#4881,#3107,.T.);
#5920=EDGE_CURVE('',#4886,#4885,#3108,.T.);
#5921=EDGE_CURVE('',#4883,#4886,#3109,.T.);
#5922=EDGE_CURVE('',#4882,#4887,#3110,.T.);
#5923=EDGE_CURVE('',#4884,#4888,#3111,.T.);
#5924=EDGE_CURVE('',#4887,#4888,#3112,.T.);
#5925=EDGE_CURVE('',#4888,#4886,#3113,.T.);
#5926=EDGE_CURVE('',#4887,#4885,#3114,.T.);
#5927=EDGE_CURVE('',#4889,#4889,#4194,.T.);
#5928=EDGE_CURVE('',#4889,#4890,#3115,.T.);
#5929=EDGE_CURVE('',#4890,#4890,#4195,.T.);
#5930=EDGE_CURVE('',#4891,#4891,#4196,.T.);
#5931=EDGE_CURVE('',#4891,#4892,#3116,.T.);
#5932=EDGE_CURVE('',#4892,#4892,#4197,.T.);
#5933=EDGE_CURVE('',#4893,#4893,#4198,.T.);
#5934=EDGE_CURVE('',#4893,#4894,#3117,.T.);
#5935=EDGE_CURVE('',#4894,#4894,#4199,.T.);
#5936=EDGE_CURVE('',#4895,#4895,#4200,.T.);
#5937=EDGE_CURVE('',#4895,#4896,#3118,.T.);
#5938=EDGE_CURVE('',#4896,#4896,#4201,.T.);
#5939=EDGE_CURVE('',#4897,#4897,#4202,.T.);
#5940=EDGE_CURVE('',#4897,#4898,#3119,.T.);
#5941=EDGE_CURVE('',#4898,#4898,#4203,.T.);
#5942=EDGE_CURVE('',#4899,#4899,#4204,.T.);
#5943=EDGE_CURVE('',#4899,#4900,#3120,.T.);
#5944=EDGE_CURVE('',#4900,#4900,#4205,.T.);
#5945=EDGE_CURVE('',#4901,#4902,#3121,.T.);
#5946=EDGE_CURVE('',#4902,#4903,#3122,.T.);
#5947=EDGE_CURVE('',#4904,#4903,#3123,.T.);
#5948=EDGE_CURVE('',#4901,#4904,#3124,.T.);
#5949=EDGE_CURVE('',#4905,#4901,#3125,.T.);
#5950=EDGE_CURVE('',#4906,#4904,#3126,.T.);
#5951=EDGE_CURVE('',#4905,#4906,#3127,.T.);
#5952=EDGE_CURVE('',#4907,#4905,#3128,.T.);
#5953=EDGE_CURVE('',#4908,#4906,#3129,.T.);
#5954=EDGE_CURVE('',#4907,#4908,#3130,.T.);
#5955=EDGE_CURVE('',#4902,#4907,#3131,.T.);
#5956=EDGE_CURVE('',#4903,#4908,#3132,.T.);
#5957=EDGE_CURVE('',#4909,#4909,#4206,.T.);
#5958=EDGE_CURVE('',#4909,#4910,#3133,.T.);
#5959=EDGE_CURVE('',#4910,#4910,#4207,.T.);
#5960=EDGE_CURVE('',#4911,#4911,#4208,.T.);
#5961=EDGE_CURVE('',#4911,#4912,#3134,.T.);
#5962=EDGE_CURVE('',#4912,#4912,#4209,.T.);
#5963=EDGE_CURVE('',#4913,#4913,#4210,.T.);
#5964=EDGE_CURVE('',#4913,#4914,#3135,.T.);
#5965=EDGE_CURVE('',#4914,#4914,#4211,.T.);
#5966=EDGE_CURVE('',#4915,#4915,#4212,.T.);
#5967=EDGE_CURVE('',#4915,#4916,#3136,.T.);
#5968=EDGE_CURVE('',#4916,#4916,#4213,.T.);
#5969=EDGE_CURVE('',#4917,#4917,#4214,.T.);
#5970=EDGE_CURVE('',#4917,#4918,#3137,.T.);
#5971=EDGE_CURVE('',#4918,#4918,#4215,.T.);
#5972=EDGE_CURVE('',#4919,#4919,#4216,.T.);
#5973=EDGE_CURVE('',#4919,#4920,#3138,.T.);
#5974=EDGE_CURVE('',#4920,#4920,#4217,.T.);
#5975=EDGE_CURVE('',#4921,#4922,#3139,.T.);
#5976=EDGE_CURVE('',#4922,#4923,#3140,.T.);
#5977=EDGE_CURVE('',#4924,#4923,#3141,.T.);
#5978=EDGE_CURVE('',#4921,#4924,#3142,.T.);
#5979=EDGE_CURVE('',#4925,#4921,#3143,.T.);
#5980=EDGE_CURVE('',#4926,#4924,#3144,.T.);
#5981=EDGE_CURVE('',#4925,#4926,#3145,.T.);
#5982=EDGE_CURVE('',#4927,#4925,#3146,.T.);
#5983=EDGE_CURVE('',#4928,#4926,#3147,.T.);
#5984=EDGE_CURVE('',#4927,#4928,#3148,.T.);
#5985=EDGE_CURVE('',#4922,#4927,#3149,.T.);
#5986=EDGE_CURVE('',#4923,#4928,#3150,.T.);
#5987=EDGE_CURVE('',#4929,#4929,#4218,.T.);
#5988=EDGE_CURVE('',#4929,#4930,#3151,.T.);
#5989=EDGE_CURVE('',#4930,#4930,#4219,.T.);
#5990=EDGE_CURVE('',#4931,#4931,#4220,.T.);
#5991=EDGE_CURVE('',#4931,#4932,#3152,.T.);
#5992=EDGE_CURVE('',#4932,#4932,#4221,.T.);
#5993=EDGE_CURVE('',#4933,#4933,#4222,.T.);
#5994=EDGE_CURVE('',#4933,#4934,#3153,.T.);
#5995=EDGE_CURVE('',#4934,#4934,#4223,.T.);
#5996=EDGE_CURVE('',#4935,#4935,#4224,.T.);
#5997=EDGE_CURVE('',#4935,#4936,#3154,.T.);
#5998=EDGE_CURVE('',#4936,#4936,#4225,.T.);
#5999=EDGE_CURVE('',#4937,#4937,#4226,.T.);
#6000=EDGE_CURVE('',#4937,#4938,#3155,.T.);
#6001=EDGE_CURVE('',#4938,#4938,#4227,.T.);
#6002=EDGE_CURVE('',#4939,#4939,#4228,.T.);
#6003=EDGE_CURVE('',#4939,#4940,#3156,.T.);
#6004=EDGE_CURVE('',#4940,#4940,#4229,.T.);
#6005=EDGE_CURVE('',#4941,#4942,#3157,.T.);
#6006=EDGE_CURVE('',#4942,#4943,#3158,.T.);
#6007=EDGE_CURVE('',#4944,#4943,#3159,.T.);
#6008=EDGE_CURVE('',#4941,#4944,#3160,.T.);
#6009=EDGE_CURVE('',#4945,#4941,#3161,.T.);
#6010=EDGE_CURVE('',#4946,#4944,#3162,.T.);
#6011=EDGE_CURVE('',#4945,#4946,#3163,.T.);
#6012=EDGE_CURVE('',#4947,#4945,#3164,.T.);
#6013=EDGE_CURVE('',#4948,#4946,#3165,.T.);
#6014=EDGE_CURVE('',#4947,#4948,#3166,.T.);
#6015=EDGE_CURVE('',#4942,#4947,#3167,.T.);
#6016=EDGE_CURVE('',#4943,#4948,#3168,.T.);
#6017=EDGE_CURVE('',#4949,#4949,#4230,.T.);
#6018=EDGE_CURVE('',#4949,#4950,#3169,.T.);
#6019=EDGE_CURVE('',#4950,#4950,#4231,.T.);
#6020=EDGE_CURVE('',#4951,#4951,#4232,.T.);
#6021=EDGE_CURVE('',#4952,#4952,#4233,.T.);
#6022=EDGE_CURVE('',#4951,#4953,#3170,.T.);
#6023=EDGE_CURVE('',#4953,#4953,#4234,.T.);
#6024=EDGE_CURVE('',#4954,#4954,#4235,.T.);
#6025=EDGE_CURVE('',#4954,#4952,#3171,.T.);
#6026=EDGE_CURVE('',#4955,#4955,#4236,.T.);
#6027=EDGE_CURVE('',#4955,#4956,#3172,.T.);
#6028=EDGE_CURVE('',#4956,#4956,#4237,.T.);
#6029=EDGE_CURVE('',#4957,#4957,#4238,.T.);
#6030=EDGE_CURVE('',#4957,#4958,#3173,.T.);
#6031=EDGE_CURVE('',#4958,#4958,#4239,.T.);
#6032=EDGE_CURVE('',#4959,#4959,#4240,.T.);
#6033=EDGE_CURVE('',#4959,#4960,#3174,.T.);
#6034=EDGE_CURVE('',#4960,#4960,#4241,.T.);
#6035=EDGE_CURVE('',#4961,#4961,#4242,.T.);
#6036=EDGE_CURVE('',#4961,#4962,#3175,.T.);
#6037=EDGE_CURVE('',#4962,#4962,#4243,.T.);
#6038=EDGE_CURVE('',#4963,#4963,#4244,.T.);
#6039=EDGE_CURVE('',#4963,#4964,#3176,.T.);
#6040=EDGE_CURVE('',#4964,#4964,#4245,.T.);
#6041=EDGE_CURVE('',#4965,#4965,#4246,.T.);
#6042=EDGE_CURVE('',#4965,#4966,#3177,.T.);
#6043=EDGE_CURVE('',#4966,#4966,#4247,.T.);
#6044=EDGE_CURVE('',#4967,#4968,#4248,.T.);
#6045=EDGE_CURVE('',#4969,#4967,#3178,.T.);
#6046=EDGE_CURVE('',#4970,#4969,#3179,.T.);
#6047=EDGE_CURVE('',#4968,#4970,#3180,.T.);
#6048=EDGE_CURVE('',#4968,#4971,#3181,.T.);
#6049=EDGE_CURVE('',#4972,#4970,#3182,.T.);
#6050=EDGE_CURVE('',#4972,#4971,#3183,.T.);
#6051=EDGE_CURVE('',#4971,#4973,#4249,.T.);
#6052=EDGE_CURVE('',#4974,#4972,#3184,.T.);
#6053=EDGE_CURVE('',#4973,#4974,#3185,.T.);
#6054=EDGE_CURVE('',#4973,#4967,#3186,.T.);
#6055=EDGE_CURVE('',#4974,#4969,#3187,.T.);
#6056=EDGE_CURVE('',#4975,#4975,#4250,.T.);
#6057=EDGE_CURVE('',#4976,#4976,#4251,.T.);
#6058=EDGE_CURVE('',#4977,#4977,#4252,.T.);
#6059=EDGE_CURVE('',#4977,#4975,#3188,.T.);
#6060=EDGE_CURVE('',#4978,#4978,#4253,.T.);
#6061=EDGE_CURVE('',#4979,#4979,#4254,.T.);
#6062=EDGE_CURVE('',#4979,#4978,#3189,.T.);
#6063=EDGE_CURVE('',#4980,#4980,#4255,.T.);
#6064=EDGE_CURVE('',#4981,#4981,#4256,.T.);
#6065=EDGE_CURVE('',#4981,#4980,#3190,.T.);
#6066=EDGE_CURVE('',#4982,#4982,#4257,.T.);
#6067=EDGE_CURVE('',#4983,#4983,#4258,.T.);
#6068=EDGE_CURVE('',#4983,#4982,#3191,.T.);
#6069=EDGE_CURVE('',#4984,#4984,#4259,.T.);
#6070=EDGE_CURVE('',#4985,#4985,#4260,.T.);
#6071=EDGE_CURVE('',#4985,#4984,#3192,.T.);
#6072=EDGE_CURVE('',#4986,#4986,#4261,.T.);
#6073=EDGE_CURVE('',#4986,#4976,#3193,.T.);
#6074=EDGE_CURVE('',#4987,#4988,#4262,.T.);
#6075=EDGE_CURVE('',#4989,#4987,#3194,.T.);
#6076=EDGE_CURVE('',#4990,#4989,#4263,.T.);
#6077=EDGE_CURVE('',#4988,#4990,#3195,.T.);
#6078=EDGE_CURVE('',#4988,#4991,#3196,.T.);
#6079=EDGE_CURVE('',#4992,#4990,#3197,.T.);
#6080=EDGE_CURVE('',#4992,#4991,#3198,.T.);
#6081=EDGE_CURVE('',#4991,#4993,#4264,.T.);
#6082=EDGE_CURVE('',#4994,#4992,#4265,.T.);
#6083=EDGE_CURVE('',#4993,#4994,#3199,.T.);
#6084=EDGE_CURVE('',#4993,#4987,#3200,.T.);
#6085=EDGE_CURVE('',#4989,#4994,#3201,.T.);
#6086=EDGE_CURVE('',#4995,#4995,#4266,.T.);
#6087=EDGE_CURVE('',#4996,#4996,#4267,.T.);
#6088=EDGE_CURVE('',#4997,#4997,#4268,.T.);
#6089=EDGE_CURVE('',#4997,#4995,#3202,.T.);
#6090=EDGE_CURVE('',#4998,#4998,#4269,.T.);
#6091=EDGE_CURVE('',#4998,#4996,#3203,.T.);
#6092=EDGE_CURVE('',#4999,#5000,#3204,.T.);
#6093=EDGE_CURVE('',#5000,#5001,#3205,.T.);
#6094=EDGE_CURVE('',#5001,#5002,#3206,.T.);
#6095=EDGE_CURVE('',#4999,#5002,#3207,.T.);
#6096=EDGE_CURVE('',#5000,#5003,#3208,.T.);
#6097=EDGE_CURVE('',#5003,#5004,#3209,.T.);
#6098=EDGE_CURVE('',#5004,#5001,#3210,.T.);
#6099=EDGE_CURVE('',#5003,#5005,#3211,.T.);
#6100=EDGE_CURVE('',#5005,#5006,#3212,.T.);
#6101=EDGE_CURVE('',#5006,#5004,#3213,.T.);
#6102=EDGE_CURVE('',#5005,#5007,#3214,.T.);
#6103=EDGE_CURVE('',#5007,#5008,#3215,.T.);
#6104=EDGE_CURVE('',#5008,#5006,#3216,.T.);
#6105=EDGE_CURVE('',#5007,#5009,#3217,.T.);
#6106=EDGE_CURVE('',#5009,#5010,#3218,.T.);
#6107=EDGE_CURVE('',#5010,#5008,#3219,.T.);
#6108=EDGE_CURVE('',#5009,#4999,#3220,.T.);
#6109=EDGE_CURVE('',#5002,#5010,#3221,.T.);
#6110=EDGE_CURVE('',#5011,#5011,#4270,.T.);
#6111=EDGE_CURVE('',#5012,#5012,#4271,.T.);
#6112=EDGE_CURVE('',#5013,#5013,#4272,.T.);
#6113=EDGE_CURVE('',#5013,#5012,#3222,.T.);
#6114=EDGE_CURVE('',#5014,#5014,#4273,.T.);
#6115=EDGE_CURVE('',#5014,#5013,#3223,.T.);
#6116=EDGE_CURVE('',#5015,#5015,#4274,.T.);
#6117=EDGE_CURVE('',#5015,#5014,#3224,.T.);
#6118=EDGE_CURVE('',#5016,#5016,#4275,.T.);
#6119=EDGE_CURVE('',#5017,#5017,#4276,.F.);
#6120=EDGE_CURVE('',#5017,#5016,#3225,.T.);
#6121=EDGE_CURVE('',#5011,#5017,#3226,.T.);
#6122=ORIENTED_EDGE('',*,*,#5018,.F.);
#6123=ORIENTED_EDGE('',*,*,#5019,.T.);
#6124=ORIENTED_EDGE('',*,*,#5020,.F.);
#6125=ORIENTED_EDGE('',*,*,#5019,.F.);
#6126=ORIENTED_EDGE('',*,*,#5021,.F.);
#6127=ORIENTED_EDGE('',*,*,#5022,.T.);
#6128=ORIENTED_EDGE('',*,*,#5023,.F.);
#6129=ORIENTED_EDGE('',*,*,#5022,.F.);
#6130=ORIENTED_EDGE('',*,*,#5024,.F.);
#6131=ORIENTED_EDGE('',*,*,#5025,.T.);
#6132=ORIENTED_EDGE('',*,*,#5026,.F.);
#6133=ORIENTED_EDGE('',*,*,#5025,.F.);
#6134=ORIENTED_EDGE('',*,*,#5027,.F.);
#6135=ORIENTED_EDGE('',*,*,#5028,.T.);
#6136=ORIENTED_EDGE('',*,*,#5029,.F.);
#6137=ORIENTED_EDGE('',*,*,#5028,.F.);
#6138=ORIENTED_EDGE('',*,*,#5030,.F.);
#6139=ORIENTED_EDGE('',*,*,#5031,.T.);
#6140=ORIENTED_EDGE('',*,*,#5032,.F.);
#6141=ORIENTED_EDGE('',*,*,#5031,.F.);
#6142=ORIENTED_EDGE('',*,*,#5033,.F.);
#6143=ORIENTED_EDGE('',*,*,#5034,.T.);
#6144=ORIENTED_EDGE('',*,*,#5035,.F.);
#6145=ORIENTED_EDGE('',*,*,#5034,.F.);
#6146=ORIENTED_EDGE('',*,*,#5036,.F.);
#6147=ORIENTED_EDGE('',*,*,#5037,.T.);
#6148=ORIENTED_EDGE('',*,*,#5038,.F.);
#6149=ORIENTED_EDGE('',*,*,#5037,.F.);
#6150=ORIENTED_EDGE('',*,*,#5039,.F.);
#6151=ORIENTED_EDGE('',*,*,#5040,.T.);
#6152=ORIENTED_EDGE('',*,*,#5041,.F.);
#6153=ORIENTED_EDGE('',*,*,#5040,.F.);
#6154=ORIENTED_EDGE('',*,*,#5042,.F.);
#6155=ORIENTED_EDGE('',*,*,#5043,.T.);
#6156=ORIENTED_EDGE('',*,*,#5044,.F.);
#6157=ORIENTED_EDGE('',*,*,#5043,.F.);
#6158=ORIENTED_EDGE('',*,*,#5045,.F.);
#6159=ORIENTED_EDGE('',*,*,#5046,.T.);
#6160=ORIENTED_EDGE('',*,*,#5047,.F.);
#6161=ORIENTED_EDGE('',*,*,#5046,.F.);
#6162=ORIENTED_EDGE('',*,*,#5048,.F.);
#6163=ORIENTED_EDGE('',*,*,#5049,.T.);
#6164=ORIENTED_EDGE('',*,*,#5050,.F.);
#6165=ORIENTED_EDGE('',*,*,#5049,.F.);
#6166=ORIENTED_EDGE('',*,*,#5051,.F.);
#6167=ORIENTED_EDGE('',*,*,#5052,.T.);
#6168=ORIENTED_EDGE('',*,*,#5053,.F.);
#6169=ORIENTED_EDGE('',*,*,#5052,.F.);
#6170=ORIENTED_EDGE('',*,*,#5054,.T.);
#6171=ORIENTED_EDGE('',*,*,#5055,.T.);
#6172=ORIENTED_EDGE('',*,*,#5056,.F.);
#6173=ORIENTED_EDGE('',*,*,#5057,.F.);
#6174=ORIENTED_EDGE('',*,*,#5058,.T.);
#6175=ORIENTED_EDGE('',*,*,#5057,.T.);
#6176=ORIENTED_EDGE('',*,*,#5059,.F.);
#6177=ORIENTED_EDGE('',*,*,#5060,.F.);
#6178=ORIENTED_EDGE('',*,*,#5061,.T.);
#6179=ORIENTED_EDGE('',*,*,#5060,.T.);
#6180=ORIENTED_EDGE('',*,*,#5062,.F.);
#6181=ORIENTED_EDGE('',*,*,#5063,.F.);
#6182=ORIENTED_EDGE('',*,*,#5064,.T.);
#6183=ORIENTED_EDGE('',*,*,#5063,.T.);
#6184=ORIENTED_EDGE('',*,*,#5065,.F.);
#6185=ORIENTED_EDGE('',*,*,#5055,.F.);
#6186=ORIENTED_EDGE('',*,*,#5065,.T.);
#6187=ORIENTED_EDGE('',*,*,#5062,.T.);
#6188=ORIENTED_EDGE('',*,*,#5059,.T.);
#6189=ORIENTED_EDGE('',*,*,#5056,.T.);
#6190=ORIENTED_EDGE('',*,*,#5026,.T.);
#6191=ORIENTED_EDGE('',*,*,#5029,.T.);
#6192=ORIENTED_EDGE('',*,*,#5053,.T.);
#6193=ORIENTED_EDGE('',*,*,#5050,.T.);
#6194=ORIENTED_EDGE('',*,*,#5047,.T.);
#6195=ORIENTED_EDGE('',*,*,#5044,.T.);
#6196=ORIENTED_EDGE('',*,*,#5041,.T.);
#6197=ORIENTED_EDGE('',*,*,#5038,.T.);
#6198=ORIENTED_EDGE('',*,*,#5035,.T.);
#6199=ORIENTED_EDGE('',*,*,#5032,.T.);
#6200=ORIENTED_EDGE('',*,*,#5023,.T.);
#6201=ORIENTED_EDGE('',*,*,#5020,.T.);
#6202=ORIENTED_EDGE('',*,*,#5064,.F.);
#6203=ORIENTED_EDGE('',*,*,#5054,.F.);
#6204=ORIENTED_EDGE('',*,*,#5058,.F.);
#6205=ORIENTED_EDGE('',*,*,#5061,.F.);
#6206=ORIENTED_EDGE('',*,*,#5024,.T.);
#6207=ORIENTED_EDGE('',*,*,#5027,.T.);
#6208=ORIENTED_EDGE('',*,*,#5051,.T.);
#6209=ORIENTED_EDGE('',*,*,#5048,.T.);
#6210=ORIENTED_EDGE('',*,*,#5045,.T.);
#6211=ORIENTED_EDGE('',*,*,#5042,.T.);
#6212=ORIENTED_EDGE('',*,*,#5039,.T.);
#6213=ORIENTED_EDGE('',*,*,#5036,.T.);
#6214=ORIENTED_EDGE('',*,*,#5033,.T.);
#6215=ORIENTED_EDGE('',*,*,#5030,.T.);
#6216=ORIENTED_EDGE('',*,*,#5021,.T.);
#6217=ORIENTED_EDGE('',*,*,#5018,.T.);
#6218=ORIENTED_EDGE('',*,*,#5066,.F.);
#6219=ORIENTED_EDGE('',*,*,#5067,.T.);
#6220=ORIENTED_EDGE('',*,*,#5068,.F.);
#6221=ORIENTED_EDGE('',*,*,#5067,.F.);
#6222=ORIENTED_EDGE('',*,*,#5066,.T.);
#6223=ORIENTED_EDGE('',*,*,#5069,.F.);
#6224=ORIENTED_EDGE('',*,*,#5070,.T.);
#6225=ORIENTED_EDGE('',*,*,#5071,.F.);
#6226=ORIENTED_EDGE('',*,*,#5070,.F.);
#6227=ORIENTED_EDGE('',*,*,#5069,.T.);
#6228=ORIENTED_EDGE('',*,*,#5072,.F.);
#6229=ORIENTED_EDGE('',*,*,#5073,.T.);
#6230=ORIENTED_EDGE('',*,*,#5074,.F.);
#6231=ORIENTED_EDGE('',*,*,#5073,.F.);
#6232=ORIENTED_EDGE('',*,*,#5072,.T.);
#6233=ORIENTED_EDGE('',*,*,#5075,.F.);
#6234=ORIENTED_EDGE('',*,*,#5076,.F.);
#6235=ORIENTED_EDGE('',*,*,#5077,.T.);
#6236=ORIENTED_EDGE('',*,*,#5078,.F.);
#6237=ORIENTED_EDGE('',*,*,#5077,.F.);
#6238=ORIENTED_EDGE('',*,*,#5076,.T.);
#6239=ORIENTED_EDGE('',*,*,#5079,.F.);
#6240=ORIENTED_EDGE('',*,*,#5080,.F.);
#6241=ORIENTED_EDGE('',*,*,#5081,.T.);
#6242=ORIENTED_EDGE('',*,*,#5082,.F.);
#6243=ORIENTED_EDGE('',*,*,#5081,.F.);
#6244=ORIENTED_EDGE('',*,*,#5080,.T.);
#6245=ORIENTED_EDGE('',*,*,#5083,.F.);
#6246=ORIENTED_EDGE('',*,*,#5084,.F.);
#6247=ORIENTED_EDGE('',*,*,#5085,.T.);
#6248=ORIENTED_EDGE('',*,*,#5086,.F.);
#6249=ORIENTED_EDGE('',*,*,#5085,.F.);
#6250=ORIENTED_EDGE('',*,*,#5084,.T.);
#6251=ORIENTED_EDGE('',*,*,#5087,.F.);
#6252=ORIENTED_EDGE('',*,*,#5088,.F.);
#6253=ORIENTED_EDGE('',*,*,#5089,.T.);
#6254=ORIENTED_EDGE('',*,*,#5075,.T.);
#6255=ORIENTED_EDGE('',*,*,#5089,.F.);
#6256=ORIENTED_EDGE('',*,*,#5090,.F.);
#6257=ORIENTED_EDGE('',*,*,#5091,.T.);
#6258=ORIENTED_EDGE('',*,*,#5079,.T.);
#6259=ORIENTED_EDGE('',*,*,#5091,.F.);
#6260=ORIENTED_EDGE('',*,*,#5092,.F.);
#6261=ORIENTED_EDGE('',*,*,#5093,.T.);
#6262=ORIENTED_EDGE('',*,*,#5083,.T.);
#6263=ORIENTED_EDGE('',*,*,#5093,.F.);
#6264=ORIENTED_EDGE('',*,*,#5094,.F.);
#6265=ORIENTED_EDGE('',*,*,#5095,.T.);
#6266=ORIENTED_EDGE('',*,*,#5087,.T.);
#6267=ORIENTED_EDGE('',*,*,#5095,.F.);
#6268=ORIENTED_EDGE('',*,*,#5096,.T.);
#6269=ORIENTED_EDGE('',*,*,#5097,.T.);
#6270=ORIENTED_EDGE('',*,*,#5098,.F.);
#6271=ORIENTED_EDGE('',*,*,#5099,.F.);
#6272=ORIENTED_EDGE('',*,*,#5100,.T.);
#6273=ORIENTED_EDGE('',*,*,#5099,.T.);
#6274=ORIENTED_EDGE('',*,*,#5101,.F.);
#6275=ORIENTED_EDGE('',*,*,#5102,.F.);
#6276=ORIENTED_EDGE('',*,*,#5103,.T.);
#6277=ORIENTED_EDGE('',*,*,#5102,.T.);
#6278=ORIENTED_EDGE('',*,*,#5104,.F.);
#6279=ORIENTED_EDGE('',*,*,#5105,.F.);
#6280=ORIENTED_EDGE('',*,*,#5106,.T.);
#6281=ORIENTED_EDGE('',*,*,#5105,.T.);
#6282=ORIENTED_EDGE('',*,*,#5107,.F.);
#6283=ORIENTED_EDGE('',*,*,#5097,.F.);
#6284=ORIENTED_EDGE('',*,*,#5107,.T.);
#6285=ORIENTED_EDGE('',*,*,#5104,.T.);
#6286=ORIENTED_EDGE('',*,*,#5101,.T.);
#6287=ORIENTED_EDGE('',*,*,#5098,.T.);
#6288=ORIENTED_EDGE('',*,*,#5068,.T.);
#6289=ORIENTED_EDGE('',*,*,#5071,.T.);
#6290=ORIENTED_EDGE('',*,*,#5086,.T.);
#6291=ORIENTED_EDGE('',*,*,#5082,.T.);
#6292=ORIENTED_EDGE('',*,*,#5078,.T.);
#6293=ORIENTED_EDGE('',*,*,#5074,.T.);
#6294=ORIENTED_EDGE('',*,*,#5106,.F.);
#6295=ORIENTED_EDGE('',*,*,#5096,.F.);
#6296=ORIENTED_EDGE('',*,*,#5100,.F.);
#6297=ORIENTED_EDGE('',*,*,#5103,.F.);
#6298=ORIENTED_EDGE('',*,*,#5088,.T.);
#6299=ORIENTED_EDGE('',*,*,#5090,.T.);
#6300=ORIENTED_EDGE('',*,*,#5092,.T.);
#6301=ORIENTED_EDGE('',*,*,#5094,.T.);
#6302=ORIENTED_EDGE('',*,*,#5108,.F.);
#6303=ORIENTED_EDGE('',*,*,#5109,.T.);
#6304=ORIENTED_EDGE('',*,*,#5110,.T.);
#6305=ORIENTED_EDGE('',*,*,#5109,.F.);
#6306=ORIENTED_EDGE('',*,*,#5111,.F.);
#6307=ORIENTED_EDGE('',*,*,#5112,.T.);
#6308=ORIENTED_EDGE('',*,*,#5113,.T.);
#6309=ORIENTED_EDGE('',*,*,#5112,.F.);
#6310=ORIENTED_EDGE('',*,*,#5111,.T.);
#6311=ORIENTED_EDGE('',*,*,#5108,.T.);
#6312=ORIENTED_EDGE('',*,*,#5113,.F.);
#6313=ORIENTED_EDGE('',*,*,#5110,.F.);
#6314=ORIENTED_EDGE('',*,*,#5114,.F.);
#6315=ORIENTED_EDGE('',*,*,#5115,.T.);
#6316=ORIENTED_EDGE('',*,*,#5116,.T.);
#6317=ORIENTED_EDGE('',*,*,#5115,.F.);
#6318=ORIENTED_EDGE('',*,*,#5117,.F.);
#6319=ORIENTED_EDGE('',*,*,#5118,.T.);
#6320=ORIENTED_EDGE('',*,*,#5119,.T.);
#6321=ORIENTED_EDGE('',*,*,#5118,.F.);
#6322=ORIENTED_EDGE('',*,*,#5117,.T.);
#6323=ORIENTED_EDGE('',*,*,#5114,.T.);
#6324=ORIENTED_EDGE('',*,*,#5119,.F.);
#6325=ORIENTED_EDGE('',*,*,#5116,.F.);
#6326=ORIENTED_EDGE('',*,*,#5120,.F.);
#6327=ORIENTED_EDGE('',*,*,#5121,.T.);
#6328=ORIENTED_EDGE('',*,*,#5122,.F.);
#6329=ORIENTED_EDGE('',*,*,#5121,.F.);
#6330=ORIENTED_EDGE('',*,*,#5120,.T.);
#6331=ORIENTED_EDGE('',*,*,#5123,.F.);
#6332=ORIENTED_EDGE('',*,*,#5124,.T.);
#6333=ORIENTED_EDGE('',*,*,#5125,.F.);
#6334=ORIENTED_EDGE('',*,*,#5124,.F.);
#6335=ORIENTED_EDGE('',*,*,#5123,.T.);
#6336=ORIENTED_EDGE('',*,*,#5126,.F.);
#6337=ORIENTED_EDGE('',*,*,#5127,.T.);
#6338=ORIENTED_EDGE('',*,*,#5128,.F.);
#6339=ORIENTED_EDGE('',*,*,#5127,.F.);
#6340=ORIENTED_EDGE('',*,*,#5126,.T.);
#6341=ORIENTED_EDGE('',*,*,#5129,.F.);
#6342=ORIENTED_EDGE('',*,*,#5130,.F.);
#6343=ORIENTED_EDGE('',*,*,#5131,.T.);
#6344=ORIENTED_EDGE('',*,*,#5132,.F.);
#6345=ORIENTED_EDGE('',*,*,#5131,.F.);
#6346=ORIENTED_EDGE('',*,*,#5130,.T.);
#6347=ORIENTED_EDGE('',*,*,#5133,.F.);
#6348=ORIENTED_EDGE('',*,*,#5134,.F.);
#6349=ORIENTED_EDGE('',*,*,#5135,.T.);
#6350=ORIENTED_EDGE('',*,*,#5136,.F.);
#6351=ORIENTED_EDGE('',*,*,#5135,.F.);
#6352=ORIENTED_EDGE('',*,*,#5134,.T.);
#6353=ORIENTED_EDGE('',*,*,#5137,.F.);
#6354=ORIENTED_EDGE('',*,*,#5138,.F.);
#6355=ORIENTED_EDGE('',*,*,#5139,.T.);
#6356=ORIENTED_EDGE('',*,*,#5140,.F.);
#6357=ORIENTED_EDGE('',*,*,#5139,.F.);
#6358=ORIENTED_EDGE('',*,*,#5138,.T.);
#6359=ORIENTED_EDGE('',*,*,#5141,.F.);
#6360=ORIENTED_EDGE('',*,*,#5142,.F.);
#6361=ORIENTED_EDGE('',*,*,#5143,.T.);
#6362=ORIENTED_EDGE('',*,*,#5129,.T.);
#6363=ORIENTED_EDGE('',*,*,#5143,.F.);
#6364=ORIENTED_EDGE('',*,*,#5144,.F.);
#6365=ORIENTED_EDGE('',*,*,#5145,.T.);
#6366=ORIENTED_EDGE('',*,*,#5133,.T.);
#6367=ORIENTED_EDGE('',*,*,#5145,.F.);
#6368=ORIENTED_EDGE('',*,*,#5146,.F.);
#6369=ORIENTED_EDGE('',*,*,#5147,.T.);
#6370=ORIENTED_EDGE('',*,*,#5137,.T.);
#6371=ORIENTED_EDGE('',*,*,#5147,.F.);
#6372=ORIENTED_EDGE('',*,*,#5148,.F.);
#6373=ORIENTED_EDGE('',*,*,#5149,.T.);
#6374=ORIENTED_EDGE('',*,*,#5141,.T.);
#6375=ORIENTED_EDGE('',*,*,#5149,.F.);
#6376=ORIENTED_EDGE('',*,*,#5150,.T.);
#6377=ORIENTED_EDGE('',*,*,#5151,.T.);
#6378=ORIENTED_EDGE('',*,*,#5152,.F.);
#6379=ORIENTED_EDGE('',*,*,#5153,.F.);
#6380=ORIENTED_EDGE('',*,*,#5154,.T.);
#6381=ORIENTED_EDGE('',*,*,#5153,.T.);
#6382=ORIENTED_EDGE('',*,*,#5155,.F.);
#6383=ORIENTED_EDGE('',*,*,#5156,.F.);
#6384=ORIENTED_EDGE('',*,*,#5157,.T.);
#6385=ORIENTED_EDGE('',*,*,#5156,.T.);
#6386=ORIENTED_EDGE('',*,*,#5158,.F.);
#6387=ORIENTED_EDGE('',*,*,#5159,.F.);
#6388=ORIENTED_EDGE('',*,*,#5160,.T.);
#6389=ORIENTED_EDGE('',*,*,#5159,.T.);
#6390=ORIENTED_EDGE('',*,*,#5161,.F.);
#6391=ORIENTED_EDGE('',*,*,#5151,.F.);
#6392=ORIENTED_EDGE('',*,*,#5161,.T.);
#6393=ORIENTED_EDGE('',*,*,#5158,.T.);
#6394=ORIENTED_EDGE('',*,*,#5155,.T.);
#6395=ORIENTED_EDGE('',*,*,#5152,.T.);
#6396=ORIENTED_EDGE('',*,*,#5122,.T.);
#6397=ORIENTED_EDGE('',*,*,#5125,.T.);
#6398=ORIENTED_EDGE('',*,*,#5140,.T.);
#6399=ORIENTED_EDGE('',*,*,#5136,.T.);
#6400=ORIENTED_EDGE('',*,*,#5132,.T.);
#6401=ORIENTED_EDGE('',*,*,#5128,.T.);
#6402=ORIENTED_EDGE('',*,*,#5160,.F.);
#6403=ORIENTED_EDGE('',*,*,#5150,.F.);
#6404=ORIENTED_EDGE('',*,*,#5154,.F.);
#6405=ORIENTED_EDGE('',*,*,#5157,.F.);
#6406=ORIENTED_EDGE('',*,*,#5142,.T.);
#6407=ORIENTED_EDGE('',*,*,#5144,.T.);
#6408=ORIENTED_EDGE('',*,*,#5146,.T.);
#6409=ORIENTED_EDGE('',*,*,#5148,.T.);
#6410=ORIENTED_EDGE('',*,*,#5162,.F.);
#6411=ORIENTED_EDGE('',*,*,#5163,.T.);
#6412=ORIENTED_EDGE('',*,*,#5164,.T.);
#6413=ORIENTED_EDGE('',*,*,#5163,.F.);
#6414=ORIENTED_EDGE('',*,*,#5165,.F.);
#6415=ORIENTED_EDGE('',*,*,#5166,.T.);
#6416=ORIENTED_EDGE('',*,*,#5167,.T.);
#6417=ORIENTED_EDGE('',*,*,#5166,.F.);
#6418=ORIENTED_EDGE('',*,*,#5165,.T.);
#6419=ORIENTED_EDGE('',*,*,#5162,.T.);
#6420=ORIENTED_EDGE('',*,*,#5167,.F.);
#6421=ORIENTED_EDGE('',*,*,#5164,.F.);
#6422=ORIENTED_EDGE('',*,*,#5168,.F.);
#6423=ORIENTED_EDGE('',*,*,#5169,.T.);
#6424=ORIENTED_EDGE('',*,*,#5170,.T.);
#6425=ORIENTED_EDGE('',*,*,#5169,.F.);
#6426=ORIENTED_EDGE('',*,*,#5171,.F.);
#6427=ORIENTED_EDGE('',*,*,#5172,.T.);
#6428=ORIENTED_EDGE('',*,*,#5173,.T.);
#6429=ORIENTED_EDGE('',*,*,#5172,.F.);
#6430=ORIENTED_EDGE('',*,*,#5171,.T.);
#6431=ORIENTED_EDGE('',*,*,#5168,.T.);
#6432=ORIENTED_EDGE('',*,*,#5173,.F.);
#6433=ORIENTED_EDGE('',*,*,#5170,.F.);
#6434=ORIENTED_EDGE('',*,*,#5174,.F.);
#6435=ORIENTED_EDGE('',*,*,#5175,.F.);
#6436=ORIENTED_EDGE('',*,*,#5176,.T.);
#6437=ORIENTED_EDGE('',*,*,#5177,.F.);
#6438=ORIENTED_EDGE('',*,*,#5178,.F.);
#6439=ORIENTED_EDGE('',*,*,#5179,.T.);
#6440=ORIENTED_EDGE('',*,*,#5180,.F.);
#6441=ORIENTED_EDGE('',*,*,#5181,.F.);
#6442=ORIENTED_EDGE('',*,*,#5178,.T.);
#6443=ORIENTED_EDGE('',*,*,#5182,.F.);
#6444=ORIENTED_EDGE('',*,*,#5174,.T.);
#6445=ORIENTED_EDGE('',*,*,#5183,.F.);
#6446=ORIENTED_EDGE('',*,*,#5184,.F.);
#6447=ORIENTED_EDGE('',*,*,#5185,.F.);
#6448=ORIENTED_EDGE('',*,*,#5175,.T.);
#6449=ORIENTED_EDGE('',*,*,#5185,.T.);
#6450=ORIENTED_EDGE('',*,*,#5186,.F.);
#6451=ORIENTED_EDGE('',*,*,#5187,.T.);
#6452=ORIENTED_EDGE('',*,*,#5180,.T.);
#6453=ORIENTED_EDGE('',*,*,#5188,.T.);
#6454=ORIENTED_EDGE('',*,*,#5189,.T.);
#6455=ORIENTED_EDGE('',*,*,#5190,.T.);
#6456=ORIENTED_EDGE('',*,*,#5183,.T.);
#6457=ORIENTED_EDGE('',*,*,#5177,.T.);
#6458=ORIENTED_EDGE('',*,*,#5191,.T.);
#6459=ORIENTED_EDGE('',*,*,#5192,.T.);
#6460=ORIENTED_EDGE('',*,*,#5193,.T.);
#6461=ORIENTED_EDGE('',*,*,#5194,.T.);
#6462=ORIENTED_EDGE('',*,*,#5195,.T.);
#6463=ORIENTED_EDGE('',*,*,#5196,.T.);
#6464=ORIENTED_EDGE('',*,*,#5197,.F.);
#6465=ORIENTED_EDGE('',*,*,#5198,.T.);
#6466=ORIENTED_EDGE('',*,*,#5182,.T.);
#6467=ORIENTED_EDGE('',*,*,#5198,.F.);
#6468=ORIENTED_EDGE('',*,*,#5199,.F.);
#6469=ORIENTED_EDGE('',*,*,#5200,.T.);
#6470=ORIENTED_EDGE('',*,*,#5186,.T.);
#6471=ORIENTED_EDGE('',*,*,#5200,.F.);
#6472=ORIENTED_EDGE('',*,*,#5201,.F.);
#6473=ORIENTED_EDGE('',*,*,#5202,.T.);
#6474=ORIENTED_EDGE('',*,*,#5196,.F.);
#6475=ORIENTED_EDGE('',*,*,#5202,.F.);
#6476=ORIENTED_EDGE('',*,*,#5201,.T.);
#6477=ORIENTED_EDGE('',*,*,#5203,.F.);
#6478=ORIENTED_EDGE('',*,*,#5204,.T.);
#6479=ORIENTED_EDGE('',*,*,#5195,.F.);
#6480=ORIENTED_EDGE('',*,*,#5204,.F.);
#6481=ORIENTED_EDGE('',*,*,#5203,.T.);
#6482=ORIENTED_EDGE('',*,*,#5205,.F.);
#6483=ORIENTED_EDGE('',*,*,#5206,.T.);
#6484=ORIENTED_EDGE('',*,*,#5194,.F.);
#6485=ORIENTED_EDGE('',*,*,#5206,.F.);
#6486=ORIENTED_EDGE('',*,*,#5205,.T.);
#6487=ORIENTED_EDGE('',*,*,#5207,.F.);
#6488=ORIENTED_EDGE('',*,*,#5208,.T.);
#6489=ORIENTED_EDGE('',*,*,#5193,.F.);
#6490=ORIENTED_EDGE('',*,*,#5208,.F.);
#6491=ORIENTED_EDGE('',*,*,#5207,.T.);
#6492=ORIENTED_EDGE('',*,*,#5209,.T.);
#6493=ORIENTED_EDGE('',*,*,#5210,.T.);
#6494=ORIENTED_EDGE('',*,*,#5192,.F.);
#6495=ORIENTED_EDGE('',*,*,#5211,.F.);
#6496=ORIENTED_EDGE('',*,*,#5212,.T.);
#6497=ORIENTED_EDGE('',*,*,#5211,.T.);
#6498=ORIENTED_EDGE('',*,*,#5191,.F.);
#6499=ORIENTED_EDGE('',*,*,#5176,.F.);
#6500=ORIENTED_EDGE('',*,*,#5184,.T.);
#6501=ORIENTED_EDGE('',*,*,#5190,.F.);
#6502=ORIENTED_EDGE('',*,*,#5213,.F.);
#6503=ORIENTED_EDGE('',*,*,#5214,.T.);
#6504=ORIENTED_EDGE('',*,*,#5213,.T.);
#6505=ORIENTED_EDGE('',*,*,#5189,.F.);
#6506=ORIENTED_EDGE('',*,*,#5215,.F.);
#6507=ORIENTED_EDGE('',*,*,#5216,.T.);
#6508=ORIENTED_EDGE('',*,*,#5215,.T.);
#6509=ORIENTED_EDGE('',*,*,#5188,.F.);
#6510=ORIENTED_EDGE('',*,*,#5179,.F.);
#6511=ORIENTED_EDGE('',*,*,#5181,.T.);
#6512=ORIENTED_EDGE('',*,*,#5187,.F.);
#6513=ORIENTED_EDGE('',*,*,#5210,.F.);
#6514=ORIENTED_EDGE('',*,*,#5216,.F.);
#6515=ORIENTED_EDGE('',*,*,#5209,.F.);
#6516=ORIENTED_EDGE('',*,*,#5212,.F.);
#6517=ORIENTED_EDGE('',*,*,#5214,.F.);
#6518=ORIENTED_EDGE('',*,*,#5197,.T.);
#6519=ORIENTED_EDGE('',*,*,#5199,.T.);
#6520=ORIENTED_EDGE('',*,*,#5217,.F.);
#6521=ORIENTED_EDGE('',*,*,#5218,.F.);
#6522=ORIENTED_EDGE('',*,*,#5219,.T.);
#6523=ORIENTED_EDGE('',*,*,#5220,.F.);
#6524=ORIENTED_EDGE('',*,*,#5221,.F.);
#6525=ORIENTED_EDGE('',*,*,#5222,.T.);
#6526=ORIENTED_EDGE('',*,*,#5223,.F.);
#6527=ORIENTED_EDGE('',*,*,#5224,.F.);
#6528=ORIENTED_EDGE('',*,*,#5221,.T.);
#6529=ORIENTED_EDGE('',*,*,#5225,.F.);
#6530=ORIENTED_EDGE('',*,*,#5217,.T.);
#6531=ORIENTED_EDGE('',*,*,#5226,.F.);
#6532=ORIENTED_EDGE('',*,*,#5227,.F.);
#6533=ORIENTED_EDGE('',*,*,#5228,.F.);
#6534=ORIENTED_EDGE('',*,*,#5218,.T.);
#6535=ORIENTED_EDGE('',*,*,#5228,.T.);
#6536=ORIENTED_EDGE('',*,*,#5229,.F.);
#6537=ORIENTED_EDGE('',*,*,#5230,.T.);
#6538=ORIENTED_EDGE('',*,*,#5223,.T.);
#6539=ORIENTED_EDGE('',*,*,#5231,.T.);
#6540=ORIENTED_EDGE('',*,*,#5232,.T.);
#6541=ORIENTED_EDGE('',*,*,#5233,.T.);
#6542=ORIENTED_EDGE('',*,*,#5226,.T.);
#6543=ORIENTED_EDGE('',*,*,#5220,.T.);
#6544=ORIENTED_EDGE('',*,*,#5234,.T.);
#6545=ORIENTED_EDGE('',*,*,#5235,.T.);
#6546=ORIENTED_EDGE('',*,*,#5236,.T.);
#6547=ORIENTED_EDGE('',*,*,#5237,.T.);
#6548=ORIENTED_EDGE('',*,*,#5238,.T.);
#6549=ORIENTED_EDGE('',*,*,#5239,.T.);
#6550=ORIENTED_EDGE('',*,*,#5240,.F.);
#6551=ORIENTED_EDGE('',*,*,#5241,.T.);
#6552=ORIENTED_EDGE('',*,*,#5225,.T.);
#6553=ORIENTED_EDGE('',*,*,#5241,.F.);
#6554=ORIENTED_EDGE('',*,*,#5242,.F.);
#6555=ORIENTED_EDGE('',*,*,#5243,.T.);
#6556=ORIENTED_EDGE('',*,*,#5229,.T.);
#6557=ORIENTED_EDGE('',*,*,#5243,.F.);
#6558=ORIENTED_EDGE('',*,*,#5244,.F.);
#6559=ORIENTED_EDGE('',*,*,#5245,.T.);
#6560=ORIENTED_EDGE('',*,*,#5239,.F.);
#6561=ORIENTED_EDGE('',*,*,#5245,.F.);
#6562=ORIENTED_EDGE('',*,*,#5244,.T.);
#6563=ORIENTED_EDGE('',*,*,#5246,.F.);
#6564=ORIENTED_EDGE('',*,*,#5247,.T.);
#6565=ORIENTED_EDGE('',*,*,#5238,.F.);
#6566=ORIENTED_EDGE('',*,*,#5247,.F.);
#6567=ORIENTED_EDGE('',*,*,#5246,.T.);
#6568=ORIENTED_EDGE('',*,*,#5248,.F.);
#6569=ORIENTED_EDGE('',*,*,#5249,.T.);
#6570=ORIENTED_EDGE('',*,*,#5237,.F.);
#6571=ORIENTED_EDGE('',*,*,#5249,.F.);
#6572=ORIENTED_EDGE('',*,*,#5248,.T.);
#6573=ORIENTED_EDGE('',*,*,#5250,.F.);
#6574=ORIENTED_EDGE('',*,*,#5251,.T.);
#6575=ORIENTED_EDGE('',*,*,#5236,.F.);
#6576=ORIENTED_EDGE('',*,*,#5251,.F.);
#6577=ORIENTED_EDGE('',*,*,#5250,.T.);
#6578=ORIENTED_EDGE('',*,*,#5252,.T.);
#6579=ORIENTED_EDGE('',*,*,#5253,.T.);
#6580=ORIENTED_EDGE('',*,*,#5235,.F.);
#6581=ORIENTED_EDGE('',*,*,#5254,.F.);
#6582=ORIENTED_EDGE('',*,*,#5255,.T.);
#6583=ORIENTED_EDGE('',*,*,#5254,.T.);
#6584=ORIENTED_EDGE('',*,*,#5234,.F.);
#6585=ORIENTED_EDGE('',*,*,#5219,.F.);
#6586=ORIENTED_EDGE('',*,*,#5227,.T.);
#6587=ORIENTED_EDGE('',*,*,#5233,.F.);
#6588=ORIENTED_EDGE('',*,*,#5256,.F.);
#6589=ORIENTED_EDGE('',*,*,#5257,.T.);
#6590=ORIENTED_EDGE('',*,*,#5256,.T.);
#6591=ORIENTED_EDGE('',*,*,#5232,.F.);
#6592=ORIENTED_EDGE('',*,*,#5258,.F.);
#6593=ORIENTED_EDGE('',*,*,#5259,.T.);
#6594=ORIENTED_EDGE('',*,*,#5258,.T.);
#6595=ORIENTED_EDGE('',*,*,#5231,.F.);
#6596=ORIENTED_EDGE('',*,*,#5222,.F.);
#6597=ORIENTED_EDGE('',*,*,#5224,.T.);
#6598=ORIENTED_EDGE('',*,*,#5230,.F.);
#6599=ORIENTED_EDGE('',*,*,#5253,.F.);
#6600=ORIENTED_EDGE('',*,*,#5259,.F.);
#6601=ORIENTED_EDGE('',*,*,#5252,.F.);
#6602=ORIENTED_EDGE('',*,*,#5255,.F.);
#6603=ORIENTED_EDGE('',*,*,#5257,.F.);
#6604=ORIENTED_EDGE('',*,*,#5240,.T.);
#6605=ORIENTED_EDGE('',*,*,#5242,.T.);
#6606=ORIENTED_EDGE('',*,*,#5260,.T.);
#6607=ORIENTED_EDGE('',*,*,#5261,.T.);
#6608=ORIENTED_EDGE('',*,*,#5262,.F.);
#6609=ORIENTED_EDGE('',*,*,#5263,.F.);
#6610=ORIENTED_EDGE('',*,*,#5264,.T.);
#6611=ORIENTED_EDGE('',*,*,#5263,.T.);
#6612=ORIENTED_EDGE('',*,*,#5265,.F.);
#6613=ORIENTED_EDGE('',*,*,#5266,.F.);
#6614=ORIENTED_EDGE('',*,*,#5267,.T.);
#6615=ORIENTED_EDGE('',*,*,#5266,.T.);
#6616=ORIENTED_EDGE('',*,*,#5268,.F.);
#6617=ORIENTED_EDGE('',*,*,#5269,.F.);
#6618=ORIENTED_EDGE('',*,*,#5270,.T.);
#6619=ORIENTED_EDGE('',*,*,#5269,.T.);
#6620=ORIENTED_EDGE('',*,*,#5271,.F.);
#6621=ORIENTED_EDGE('',*,*,#5261,.F.);
#6622=ORIENTED_EDGE('',*,*,#5271,.T.);
#6623=ORIENTED_EDGE('',*,*,#5268,.T.);
#6624=ORIENTED_EDGE('',*,*,#5265,.T.);
#6625=ORIENTED_EDGE('',*,*,#5262,.T.);
#6626=ORIENTED_EDGE('',*,*,#5270,.F.);
#6627=ORIENTED_EDGE('',*,*,#5260,.F.);
#6628=ORIENTED_EDGE('',*,*,#5264,.F.);
#6629=ORIENTED_EDGE('',*,*,#5267,.F.);
#6630=ORIENTED_EDGE('',*,*,#5272,.T.);
#6631=ORIENTED_EDGE('',*,*,#5273,.T.);
#6632=ORIENTED_EDGE('',*,*,#5274,.F.);
#6633=ORIENTED_EDGE('',*,*,#5275,.F.);
#6634=ORIENTED_EDGE('',*,*,#5276,.T.);
#6635=ORIENTED_EDGE('',*,*,#5275,.T.);
#6636=ORIENTED_EDGE('',*,*,#5277,.F.);
#6637=ORIENTED_EDGE('',*,*,#5278,.F.);
#6638=ORIENTED_EDGE('',*,*,#5279,.T.);
#6639=ORIENTED_EDGE('',*,*,#5278,.T.);
#6640=ORIENTED_EDGE('',*,*,#5280,.F.);
#6641=ORIENTED_EDGE('',*,*,#5281,.F.);
#6642=ORIENTED_EDGE('',*,*,#5282,.T.);
#6643=ORIENTED_EDGE('',*,*,#5281,.T.);
#6644=ORIENTED_EDGE('',*,*,#5283,.F.);
#6645=ORIENTED_EDGE('',*,*,#5273,.F.);
#6646=ORIENTED_EDGE('',*,*,#5283,.T.);
#6647=ORIENTED_EDGE('',*,*,#5280,.T.);
#6648=ORIENTED_EDGE('',*,*,#5277,.T.);
#6649=ORIENTED_EDGE('',*,*,#5274,.T.);
#6650=ORIENTED_EDGE('',*,*,#5282,.F.);
#6651=ORIENTED_EDGE('',*,*,#5272,.F.);
#6652=ORIENTED_EDGE('',*,*,#5276,.F.);
#6653=ORIENTED_EDGE('',*,*,#5279,.F.);
#6654=ORIENTED_EDGE('',*,*,#5284,.F.);
#6655=ORIENTED_EDGE('',*,*,#5285,.F.);
#6656=ORIENTED_EDGE('',*,*,#5286,.T.);
#6657=ORIENTED_EDGE('',*,*,#5284,.T.);
#6658=ORIENTED_EDGE('',*,*,#5286,.F.);
#6659=ORIENTED_EDGE('',*,*,#5287,.F.);
#6660=ORIENTED_EDGE('',*,*,#5288,.T.);
#6661=ORIENTED_EDGE('',*,*,#5285,.T.);
#6662=ORIENTED_EDGE('',*,*,#5288,.F.);
#6663=ORIENTED_EDGE('',*,*,#5289,.F.);
#6664=ORIENTED_EDGE('',*,*,#5290,.T.);
#6665=ORIENTED_EDGE('',*,*,#5287,.T.);
#6666=ORIENTED_EDGE('',*,*,#5290,.F.);
#6667=ORIENTED_EDGE('',*,*,#5289,.T.);
#6668=ORIENTED_EDGE('',*,*,#5291,.F.);
#6669=ORIENTED_EDGE('',*,*,#5292,.F.);
#6670=ORIENTED_EDGE('',*,*,#5293,.T.);
#6671=ORIENTED_EDGE('',*,*,#5291,.T.);
#6672=ORIENTED_EDGE('',*,*,#5293,.F.);
#6673=ORIENTED_EDGE('',*,*,#5294,.F.);
#6674=ORIENTED_EDGE('',*,*,#5295,.T.);
#6675=ORIENTED_EDGE('',*,*,#5292,.T.);
#6676=ORIENTED_EDGE('',*,*,#5295,.F.);
#6677=ORIENTED_EDGE('',*,*,#5296,.F.);
#6678=ORIENTED_EDGE('',*,*,#5297,.T.);
#6679=ORIENTED_EDGE('',*,*,#5294,.T.);
#6680=ORIENTED_EDGE('',*,*,#5297,.F.);
#6681=ORIENTED_EDGE('',*,*,#5296,.T.);
#6682=ORIENTED_EDGE('',*,*,#5298,.T.);
#6683=ORIENTED_EDGE('',*,*,#5299,.T.);
#6684=ORIENTED_EDGE('',*,*,#5300,.T.);
#6685=ORIENTED_EDGE('',*,*,#5301,.F.);
#6686=ORIENTED_EDGE('',*,*,#5302,.T.);
#6687=ORIENTED_EDGE('',*,*,#5303,.T.);
#6688=ORIENTED_EDGE('',*,*,#5304,.T.);
#6689=ORIENTED_EDGE('',*,*,#5299,.F.);
#6690=ORIENTED_EDGE('',*,*,#5305,.T.);
#6691=ORIENTED_EDGE('',*,*,#5306,.T.);
#6692=ORIENTED_EDGE('',*,*,#5307,.T.);
#6693=ORIENTED_EDGE('',*,*,#5303,.F.);
#6694=ORIENTED_EDGE('',*,*,#5308,.T.);
#6695=ORIENTED_EDGE('',*,*,#5309,.T.);
#6696=ORIENTED_EDGE('',*,*,#5310,.T.);
#6697=ORIENTED_EDGE('',*,*,#5306,.F.);
#6698=ORIENTED_EDGE('',*,*,#5311,.T.);
#6699=ORIENTED_EDGE('',*,*,#5312,.T.);
#6700=ORIENTED_EDGE('',*,*,#5313,.T.);
#6701=ORIENTED_EDGE('',*,*,#5309,.F.);
#6702=ORIENTED_EDGE('',*,*,#5314,.T.);
#6703=ORIENTED_EDGE('',*,*,#5301,.T.);
#6704=ORIENTED_EDGE('',*,*,#5315,.T.);
#6705=ORIENTED_EDGE('',*,*,#5312,.F.);
#6706=ORIENTED_EDGE('',*,*,#5314,.F.);
#6707=ORIENTED_EDGE('',*,*,#5311,.F.);
#6708=ORIENTED_EDGE('',*,*,#5308,.F.);
#6709=ORIENTED_EDGE('',*,*,#5305,.F.);
#6710=ORIENTED_EDGE('',*,*,#5302,.F.);
#6711=ORIENTED_EDGE('',*,*,#5298,.F.);
#6712=ORIENTED_EDGE('',*,*,#5315,.F.);
#6713=ORIENTED_EDGE('',*,*,#5300,.F.);
#6714=ORIENTED_EDGE('',*,*,#5304,.F.);
#6715=ORIENTED_EDGE('',*,*,#5307,.F.);
#6716=ORIENTED_EDGE('',*,*,#5310,.F.);
#6717=ORIENTED_EDGE('',*,*,#5313,.F.);
#6718=ORIENTED_EDGE('',*,*,#5316,.F.);
#6719=ORIENTED_EDGE('',*,*,#5317,.T.);
#6720=ORIENTED_EDGE('',*,*,#5318,.F.);
#6721=ORIENTED_EDGE('',*,*,#5317,.F.);
#6722=ORIENTED_EDGE('',*,*,#5319,.F.);
#6723=ORIENTED_EDGE('',*,*,#5320,.T.);
#6724=ORIENTED_EDGE('',*,*,#5321,.F.);
#6725=ORIENTED_EDGE('',*,*,#5320,.F.);
#6726=ORIENTED_EDGE('',*,*,#5322,.T.);
#6727=ORIENTED_EDGE('',*,*,#5322,.F.);
#6728=ORIENTED_EDGE('',*,*,#5319,.T.);
#6729=ORIENTED_EDGE('',*,*,#5318,.T.);
#6730=ORIENTED_EDGE('',*,*,#5323,.F.);
#6731=ORIENTED_EDGE('',*,*,#5324,.T.);
#6732=ORIENTED_EDGE('',*,*,#5325,.F.);
#6733=ORIENTED_EDGE('',*,*,#5326,.F.);
#6734=ORIENTED_EDGE('',*,*,#5327,.F.);
#6735=ORIENTED_EDGE('',*,*,#5328,.T.);
#6736=ORIENTED_EDGE('',*,*,#5329,.F.);
#6737=ORIENTED_EDGE('',*,*,#5330,.F.);
#6738=ORIENTED_EDGE('',*,*,#5331,.T.);
#6739=ORIENTED_EDGE('',*,*,#5332,.F.);
#6740=ORIENTED_EDGE('',*,*,#5331,.F.);
#6741=ORIENTED_EDGE('',*,*,#5333,.F.);
#6742=ORIENTED_EDGE('',*,*,#5324,.F.);
#6743=ORIENTED_EDGE('',*,*,#5334,.F.);
#6744=ORIENTED_EDGE('',*,*,#5335,.T.);
#6745=ORIENTED_EDGE('',*,*,#5336,.F.);
#6746=ORIENTED_EDGE('',*,*,#5337,.F.);
#6747=ORIENTED_EDGE('',*,*,#5328,.F.);
#6748=ORIENTED_EDGE('',*,*,#5338,.F.);
#6749=ORIENTED_EDGE('',*,*,#5335,.F.);
#6750=ORIENTED_EDGE('',*,*,#5339,.T.);
#6751=ORIENTED_EDGE('',*,*,#5340,.T.);
#6752=ORIENTED_EDGE('',*,*,#5341,.T.);
#6753=ORIENTED_EDGE('',*,*,#5342,.T.);
#6754=ORIENTED_EDGE('',*,*,#5343,.T.);
#6755=ORIENTED_EDGE('',*,*,#5344,.T.);
#6756=ORIENTED_EDGE('',*,*,#5326,.T.);
#6757=ORIENTED_EDGE('',*,*,#5337,.T.);
#6758=ORIENTED_EDGE('',*,*,#5334,.T.);
#6759=ORIENTED_EDGE('',*,*,#5345,.T.);
#6760=ORIENTED_EDGE('',*,*,#5346,.T.);
#6761=ORIENTED_EDGE('',*,*,#5347,.T.);
#6762=ORIENTED_EDGE('',*,*,#5329,.T.);
#6763=ORIENTED_EDGE('',*,*,#5332,.T.);
#6764=ORIENTED_EDGE('',*,*,#5323,.T.);
#6765=ORIENTED_EDGE('',*,*,#5348,.T.);
#6766=ORIENTED_EDGE('',*,*,#5349,.T.);
#6767=ORIENTED_EDGE('',*,*,#5350,.T.);
#6768=ORIENTED_EDGE('',*,*,#5327,.T.);
#6769=ORIENTED_EDGE('',*,*,#5350,.F.);
#6770=ORIENTED_EDGE('',*,*,#5351,.F.);
#6771=ORIENTED_EDGE('',*,*,#5348,.F.);
#6772=ORIENTED_EDGE('',*,*,#5325,.T.);
#6773=ORIENTED_EDGE('',*,*,#5333,.T.);
#6774=ORIENTED_EDGE('',*,*,#5330,.T.);
#6775=ORIENTED_EDGE('',*,*,#5347,.F.);
#6776=ORIENTED_EDGE('',*,*,#5352,.F.);
#6777=ORIENTED_EDGE('',*,*,#5345,.F.);
#6778=ORIENTED_EDGE('',*,*,#5336,.T.);
#6779=ORIENTED_EDGE('',*,*,#5338,.T.);
#6780=ORIENTED_EDGE('',*,*,#5346,.F.);
#6781=ORIENTED_EDGE('',*,*,#5352,.T.);
#6782=ORIENTED_EDGE('',*,*,#5316,.T.);
#6783=ORIENTED_EDGE('',*,*,#5349,.F.);
#6784=ORIENTED_EDGE('',*,*,#5351,.T.);
#6785=ORIENTED_EDGE('',*,*,#5321,.T.);
#6786=ORIENTED_EDGE('',*,*,#5353,.F.);
#6787=ORIENTED_EDGE('',*,*,#5354,.T.);
#6788=ORIENTED_EDGE('',*,*,#5355,.T.);
#6789=ORIENTED_EDGE('',*,*,#5356,.F.);
#6790=ORIENTED_EDGE('',*,*,#5357,.F.);
#6791=ORIENTED_EDGE('',*,*,#5358,.T.);
#6792=ORIENTED_EDGE('',*,*,#5359,.T.);
#6793=ORIENTED_EDGE('',*,*,#5354,.F.);
#6794=ORIENTED_EDGE('',*,*,#5360,.F.);
#6795=ORIENTED_EDGE('',*,*,#5361,.T.);
#6796=ORIENTED_EDGE('',*,*,#5362,.T.);
#6797=ORIENTED_EDGE('',*,*,#5358,.F.);
#6798=ORIENTED_EDGE('',*,*,#5363,.F.);
#6799=ORIENTED_EDGE('',*,*,#5356,.T.);
#6800=ORIENTED_EDGE('',*,*,#5364,.T.);
#6801=ORIENTED_EDGE('',*,*,#5361,.F.);
#6802=ORIENTED_EDGE('',*,*,#5364,.F.);
#6803=ORIENTED_EDGE('',*,*,#5355,.F.);
#6804=ORIENTED_EDGE('',*,*,#5359,.F.);
#6805=ORIENTED_EDGE('',*,*,#5362,.F.);
#6806=ORIENTED_EDGE('',*,*,#5365,.F.);
#6807=ORIENTED_EDGE('',*,*,#5366,.T.);
#6808=ORIENTED_EDGE('',*,*,#5344,.F.);
#6809=ORIENTED_EDGE('',*,*,#5366,.F.);
#6810=ORIENTED_EDGE('',*,*,#5367,.F.);
#6811=ORIENTED_EDGE('',*,*,#5368,.T.);
#6812=ORIENTED_EDGE('',*,*,#5343,.F.);
#6813=ORIENTED_EDGE('',*,*,#5368,.F.);
#6814=ORIENTED_EDGE('',*,*,#5369,.T.);
#6815=ORIENTED_EDGE('',*,*,#5370,.T.);
#6816=ORIENTED_EDGE('',*,*,#5342,.F.);
#6817=ORIENTED_EDGE('',*,*,#5371,.F.);
#6818=ORIENTED_EDGE('',*,*,#5372,.T.);
#6819=ORIENTED_EDGE('',*,*,#5371,.T.);
#6820=ORIENTED_EDGE('',*,*,#5341,.F.);
#6821=ORIENTED_EDGE('',*,*,#5373,.F.);
#6822=ORIENTED_EDGE('',*,*,#5374,.T.);
#6823=ORIENTED_EDGE('',*,*,#5373,.T.);
#6824=ORIENTED_EDGE('',*,*,#5340,.F.);
#6825=ORIENTED_EDGE('',*,*,#5375,.F.);
#6826=ORIENTED_EDGE('',*,*,#5376,.T.);
#6827=ORIENTED_EDGE('',*,*,#5375,.T.);
#6828=ORIENTED_EDGE('',*,*,#5339,.F.);
#6829=ORIENTED_EDGE('',*,*,#5370,.F.);
#6830=ORIENTED_EDGE('',*,*,#5376,.F.);
#6831=ORIENTED_EDGE('',*,*,#5369,.F.);
#6832=ORIENTED_EDGE('',*,*,#5372,.F.);
#6833=ORIENTED_EDGE('',*,*,#5374,.F.);
#6834=ORIENTED_EDGE('',*,*,#5353,.T.);
#6835=ORIENTED_EDGE('',*,*,#5363,.T.);
#6836=ORIENTED_EDGE('',*,*,#5360,.T.);
#6837=ORIENTED_EDGE('',*,*,#5357,.T.);
#6838=ORIENTED_EDGE('',*,*,#5365,.T.);
#6839=ORIENTED_EDGE('',*,*,#5367,.T.);
#6840=ORIENTED_EDGE('',*,*,#5377,.T.);
#6841=ORIENTED_EDGE('',*,*,#5378,.T.);
#6842=ORIENTED_EDGE('',*,*,#5379,.F.);
#6843=ORIENTED_EDGE('',*,*,#5378,.F.);
#6844=ORIENTED_EDGE('',*,*,#5380,.F.);
#6845=ORIENTED_EDGE('',*,*,#5379,.T.);
#6846=ORIENTED_EDGE('',*,*,#5381,.T.);
#6847=ORIENTED_EDGE('',*,*,#5381,.F.);
#6848=ORIENTED_EDGE('',*,*,#5380,.T.);
#6849=ORIENTED_EDGE('',*,*,#5382,.F.);
#6850=ORIENTED_EDGE('',*,*,#5382,.T.);
#6851=ORIENTED_EDGE('',*,*,#5377,.F.);
#6852=ORIENTED_EDGE('',*,*,#5383,.F.);
#6853=ORIENTED_EDGE('',*,*,#5384,.F.);
#6854=ORIENTED_EDGE('',*,*,#5385,.F.);
#6855=ORIENTED_EDGE('',*,*,#5386,.T.);
#6856=ORIENTED_EDGE('',*,*,#5387,.F.);
#6857=ORIENTED_EDGE('',*,*,#5386,.F.);
#6858=ORIENTED_EDGE('',*,*,#5388,.F.);
#6859=ORIENTED_EDGE('',*,*,#5389,.T.);
#6860=ORIENTED_EDGE('',*,*,#5390,.F.);
#6861=ORIENTED_EDGE('',*,*,#5391,.F.);
#6862=ORIENTED_EDGE('',*,*,#5392,.F.);
#6863=ORIENTED_EDGE('',*,*,#5389,.F.);
#6864=ORIENTED_EDGE('',*,*,#5393,.F.);
#6865=ORIENTED_EDGE('',*,*,#5394,.T.);
#6866=ORIENTED_EDGE('',*,*,#5395,.T.);
#6867=ORIENTED_EDGE('',*,*,#5394,.F.);
#6868=ORIENTED_EDGE('',*,*,#5384,.T.);
#6869=ORIENTED_EDGE('',*,*,#5383,.T.);
#6870=ORIENTED_EDGE('',*,*,#5385,.T.);
#6871=ORIENTED_EDGE('',*,*,#5391,.T.);
#6872=ORIENTED_EDGE('',*,*,#5390,.T.);
#6873=ORIENTED_EDGE('',*,*,#5392,.T.);
#6874=ORIENTED_EDGE('',*,*,#5396,.T.);
#6875=ORIENTED_EDGE('',*,*,#5397,.T.);
#6876=ORIENTED_EDGE('',*,*,#5398,.T.);
#6877=ORIENTED_EDGE('',*,*,#5399,.T.);
#6878=ORIENTED_EDGE('',*,*,#5400,.T.);
#6879=ORIENTED_EDGE('',*,*,#5401,.T.);
#6880=ORIENTED_EDGE('',*,*,#5402,.T.);
#6881=ORIENTED_EDGE('',*,*,#5403,.T.);
#6882=ORIENTED_EDGE('',*,*,#5404,.T.);
#6883=ORIENTED_EDGE('',*,*,#5405,.T.);
#6884=ORIENTED_EDGE('',*,*,#5406,.T.);
#6885=ORIENTED_EDGE('',*,*,#5407,.T.);
#6886=ORIENTED_EDGE('',*,*,#5397,.F.);
#6887=ORIENTED_EDGE('',*,*,#5396,.F.);
#6888=ORIENTED_EDGE('',*,*,#5398,.F.);
#6889=ORIENTED_EDGE('',*,*,#5408,.T.);
#6890=ORIENTED_EDGE('',*,*,#5409,.F.);
#6891=ORIENTED_EDGE('',*,*,#5408,.F.);
#6892=ORIENTED_EDGE('',*,*,#5410,.F.);
#6893=ORIENTED_EDGE('',*,*,#5411,.T.);
#6894=ORIENTED_EDGE('',*,*,#5400,.F.);
#6895=ORIENTED_EDGE('',*,*,#5399,.F.);
#6896=ORIENTED_EDGE('',*,*,#5401,.F.);
#6897=ORIENTED_EDGE('',*,*,#5411,.F.);
#6898=ORIENTED_EDGE('',*,*,#5403,.F.);
#6899=ORIENTED_EDGE('',*,*,#5402,.F.);
#6900=ORIENTED_EDGE('',*,*,#5404,.F.);
#6901=ORIENTED_EDGE('',*,*,#5412,.T.);
#6902=ORIENTED_EDGE('',*,*,#5413,.F.);
#6903=ORIENTED_EDGE('',*,*,#5412,.F.);
#6904=ORIENTED_EDGE('',*,*,#5414,.F.);
#6905=ORIENTED_EDGE('',*,*,#5415,.T.);
#6906=ORIENTED_EDGE('',*,*,#5406,.F.);
#6907=ORIENTED_EDGE('',*,*,#5405,.F.);
#6908=ORIENTED_EDGE('',*,*,#5407,.F.);
#6909=ORIENTED_EDGE('',*,*,#5415,.F.);
#6910=ORIENTED_EDGE('',*,*,#5395,.F.);
#6911=ORIENTED_EDGE('',*,*,#5416,.T.);
#6912=ORIENTED_EDGE('',*,*,#5417,.F.);
#6913=ORIENTED_EDGE('',*,*,#5393,.T.);
#6914=ORIENTED_EDGE('',*,*,#5418,.F.);
#6915=ORIENTED_EDGE('',*,*,#5419,.T.);
#6916=ORIENTED_EDGE('',*,*,#5417,.T.);
#6917=ORIENTED_EDGE('',*,*,#5419,.F.);
#6918=ORIENTED_EDGE('',*,*,#5418,.T.);
#6919=ORIENTED_EDGE('',*,*,#5420,.F.);
#6920=ORIENTED_EDGE('',*,*,#5420,.T.);
#6921=ORIENTED_EDGE('',*,*,#5421,.T.);
#6922=ORIENTED_EDGE('',*,*,#5416,.F.);
#6923=ORIENTED_EDGE('',*,*,#5421,.F.);
#6924=ORIENTED_EDGE('',*,*,#5388,.T.);
#6925=ORIENTED_EDGE('',*,*,#5387,.T.);
#6926=ORIENTED_EDGE('',*,*,#5410,.T.);
#6927=ORIENTED_EDGE('',*,*,#5409,.T.);
#6928=ORIENTED_EDGE('',*,*,#5414,.T.);
#6929=ORIENTED_EDGE('',*,*,#5413,.T.);
#6930=ORIENTED_EDGE('',*,*,#5422,.F.);
#6931=ORIENTED_EDGE('',*,*,#5423,.T.);
#6932=ORIENTED_EDGE('',*,*,#5424,.T.);
#6933=ORIENTED_EDGE('',*,*,#5423,.F.);
#6934=ORIENTED_EDGE('',*,*,#5425,.F.);
#6935=ORIENTED_EDGE('',*,*,#5426,.T.);
#6936=ORIENTED_EDGE('',*,*,#5427,.T.);
#6937=ORIENTED_EDGE('',*,*,#5426,.F.);
#6938=ORIENTED_EDGE('',*,*,#5425,.T.);
#6939=ORIENTED_EDGE('',*,*,#5422,.T.);
#6940=ORIENTED_EDGE('',*,*,#5427,.F.);
#6941=ORIENTED_EDGE('',*,*,#5424,.F.);
#6942=ORIENTED_EDGE('',*,*,#5428,.T.);
#6943=ORIENTED_EDGE('',*,*,#5429,.T.);
#6944=ORIENTED_EDGE('',*,*,#5430,.T.);
#6945=ORIENTED_EDGE('',*,*,#5431,.F.);
#6946=ORIENTED_EDGE('',*,*,#5432,.T.);
#6947=ORIENTED_EDGE('',*,*,#5433,.T.);
#6948=ORIENTED_EDGE('',*,*,#5434,.T.);
#6949=ORIENTED_EDGE('',*,*,#5429,.F.);
#6950=ORIENTED_EDGE('',*,*,#5435,.T.);
#6951=ORIENTED_EDGE('',*,*,#5436,.T.);
#6952=ORIENTED_EDGE('',*,*,#5437,.T.);
#6953=ORIENTED_EDGE('',*,*,#5433,.F.);
#6954=ORIENTED_EDGE('',*,*,#5438,.T.);
#6955=ORIENTED_EDGE('',*,*,#5439,.T.);
#6956=ORIENTED_EDGE('',*,*,#5440,.T.);
#6957=ORIENTED_EDGE('',*,*,#5436,.F.);
#6958=ORIENTED_EDGE('',*,*,#5441,.T.);
#6959=ORIENTED_EDGE('',*,*,#5442,.T.);
#6960=ORIENTED_EDGE('',*,*,#5443,.T.);
#6961=ORIENTED_EDGE('',*,*,#5439,.F.);
#6962=ORIENTED_EDGE('',*,*,#5444,.T.);
#6963=ORIENTED_EDGE('',*,*,#5431,.T.);
#6964=ORIENTED_EDGE('',*,*,#5445,.T.);
#6965=ORIENTED_EDGE('',*,*,#5442,.F.);
#6966=ORIENTED_EDGE('',*,*,#5444,.F.);
#6967=ORIENTED_EDGE('',*,*,#5441,.F.);
#6968=ORIENTED_EDGE('',*,*,#5438,.F.);
#6969=ORIENTED_EDGE('',*,*,#5435,.F.);
#6970=ORIENTED_EDGE('',*,*,#5432,.F.);
#6971=ORIENTED_EDGE('',*,*,#5428,.F.);
#6972=ORIENTED_EDGE('',*,*,#5445,.F.);
#6973=ORIENTED_EDGE('',*,*,#5430,.F.);
#6974=ORIENTED_EDGE('',*,*,#5434,.F.);
#6975=ORIENTED_EDGE('',*,*,#5437,.F.);
#6976=ORIENTED_EDGE('',*,*,#5440,.F.);
#6977=ORIENTED_EDGE('',*,*,#5443,.F.);
#6978=ORIENTED_EDGE('',*,*,#5446,.F.);
#6979=ORIENTED_EDGE('',*,*,#5447,.F.);
#6980=ORIENTED_EDGE('',*,*,#5448,.F.);
#6981=ORIENTED_EDGE('',*,*,#5449,.T.);
#6982=ORIENTED_EDGE('',*,*,#5447,.T.);
#6983=ORIENTED_EDGE('',*,*,#5449,.F.);
#6984=ORIENTED_EDGE('',*,*,#5450,.F.);
#6985=ORIENTED_EDGE('',*,*,#5451,.T.);
#6986=ORIENTED_EDGE('',*,*,#5448,.T.);
#6987=ORIENTED_EDGE('',*,*,#5451,.F.);
#6988=ORIENTED_EDGE('',*,*,#5452,.F.);
#6989=ORIENTED_EDGE('',*,*,#5453,.T.);
#6990=ORIENTED_EDGE('',*,*,#5450,.T.);
#6991=ORIENTED_EDGE('',*,*,#5453,.F.);
#6992=ORIENTED_EDGE('',*,*,#5452,.T.);
#6993=ORIENTED_EDGE('',*,*,#5454,.F.);
#6994=ORIENTED_EDGE('',*,*,#5455,.F.);
#6995=ORIENTED_EDGE('',*,*,#5456,.T.);
#6996=ORIENTED_EDGE('',*,*,#5454,.T.);
#6997=ORIENTED_EDGE('',*,*,#5456,.F.);
#6998=ORIENTED_EDGE('',*,*,#5446,.T.);
#6999=ORIENTED_EDGE('',*,*,#5457,.T.);
#7000=ORIENTED_EDGE('',*,*,#5455,.T.);
#7001=ORIENTED_EDGE('',*,*,#5457,.F.);
#7002=ORIENTED_EDGE('',*,*,#5458,.F.);
#7003=ORIENTED_EDGE('',*,*,#5459,.F.);
#7004=ORIENTED_EDGE('',*,*,#5460,.F.);
#7005=ORIENTED_EDGE('',*,*,#5461,.F.);
#7006=ORIENTED_EDGE('',*,*,#5462,.F.);
#7007=ORIENTED_EDGE('',*,*,#5459,.T.);
#7008=ORIENTED_EDGE('',*,*,#5463,.F.);
#7009=ORIENTED_EDGE('',*,*,#5464,.T.);
#7010=ORIENTED_EDGE('',*,*,#5465,.F.);
#7011=ORIENTED_EDGE('',*,*,#5466,.F.);
#7012=ORIENTED_EDGE('',*,*,#5467,.F.);
#7013=ORIENTED_EDGE('',*,*,#5464,.F.);
#7014=ORIENTED_EDGE('',*,*,#5468,.T.);
#7015=ORIENTED_EDGE('',*,*,#5469,.F.);
#7016=ORIENTED_EDGE('',*,*,#5470,.T.);
#7017=ORIENTED_EDGE('',*,*,#5471,.F.);
#7018=ORIENTED_EDGE('',*,*,#5472,.T.);
#7019=ORIENTED_EDGE('',*,*,#5461,.T.);
#7020=ORIENTED_EDGE('',*,*,#5473,.T.);
#7021=ORIENTED_EDGE('',*,*,#5460,.T.);
#7022=ORIENTED_EDGE('',*,*,#5458,.T.);
#7023=ORIENTED_EDGE('',*,*,#5462,.T.);
#7024=ORIENTED_EDGE('',*,*,#5472,.F.);
#7025=ORIENTED_EDGE('',*,*,#5474,.F.);
#7026=ORIENTED_EDGE('',*,*,#5475,.T.);
#7027=ORIENTED_EDGE('',*,*,#5476,.F.);
#7028=ORIENTED_EDGE('',*,*,#5468,.F.);
#7029=ORIENTED_EDGE('',*,*,#5477,.T.);
#7030=ORIENTED_EDGE('',*,*,#5478,.T.);
#7031=ORIENTED_EDGE('',*,*,#5479,.F.);
#7032=ORIENTED_EDGE('',*,*,#5480,.F.);
#7033=ORIENTED_EDGE('',*,*,#5466,.T.);
#7034=ORIENTED_EDGE('',*,*,#5481,.F.);
#7035=ORIENTED_EDGE('',*,*,#5482,.F.);
#7036=ORIENTED_EDGE('',*,*,#5483,.T.);
#7037=ORIENTED_EDGE('',*,*,#5484,.F.);
#7038=ORIENTED_EDGE('',*,*,#5485,.T.);
#7039=ORIENTED_EDGE('',*,*,#5486,.F.);
#7040=ORIENTED_EDGE('',*,*,#5485,.F.);
#7041=ORIENTED_EDGE('',*,*,#5477,.F.);
#7042=ORIENTED_EDGE('',*,*,#5487,.T.);
#7043=ORIENTED_EDGE('',*,*,#5488,.F.);
#7044=ORIENTED_EDGE('',*,*,#5487,.F.);
#7045=ORIENTED_EDGE('',*,*,#5489,.F.);
#7046=ORIENTED_EDGE('',*,*,#5490,.T.);
#7047=ORIENTED_EDGE('',*,*,#5473,.F.);
#7048=ORIENTED_EDGE('',*,*,#5490,.F.);
#7049=ORIENTED_EDGE('',*,*,#5491,.F.);
#7050=ORIENTED_EDGE('',*,*,#5492,.T.);
#7051=ORIENTED_EDGE('',*,*,#5483,.F.);
#7052=ORIENTED_EDGE('',*,*,#5492,.F.);
#7053=ORIENTED_EDGE('',*,*,#5493,.F.);
#7054=ORIENTED_EDGE('',*,*,#5494,.T.);
#7055=ORIENTED_EDGE('',*,*,#5495,.F.);
#7056=ORIENTED_EDGE('',*,*,#5494,.F.);
#7057=ORIENTED_EDGE('',*,*,#5471,.T.);
#7058=ORIENTED_EDGE('',*,*,#5496,.T.);
#7059=ORIENTED_EDGE('',*,*,#5497,.T.);
#7060=ORIENTED_EDGE('',*,*,#5498,.T.);
#7061=ORIENTED_EDGE('',*,*,#5482,.T.);
#7062=ORIENTED_EDGE('',*,*,#5499,.T.);
#7063=ORIENTED_EDGE('',*,*,#5500,.T.);
#7064=ORIENTED_EDGE('',*,*,#5501,.T.);
#7065=ORIENTED_EDGE('',*,*,#5502,.T.);
#7066=ORIENTED_EDGE('',*,*,#5503,.T.);
#7067=ORIENTED_EDGE('',*,*,#5504,.T.);
#7068=ORIENTED_EDGE('',*,*,#5474,.T.);
#7069=ORIENTED_EDGE('',*,*,#5493,.T.);
#7070=ORIENTED_EDGE('',*,*,#5470,.F.);
#7071=ORIENTED_EDGE('',*,*,#5505,.F.);
#7072=ORIENTED_EDGE('',*,*,#5506,.F.);
#7073=ORIENTED_EDGE('',*,*,#5496,.F.);
#7074=ORIENTED_EDGE('',*,*,#5506,.T.);
#7075=ORIENTED_EDGE('',*,*,#5507,.F.);
#7076=ORIENTED_EDGE('',*,*,#5508,.F.);
#7077=ORIENTED_EDGE('',*,*,#5497,.F.);
#7078=ORIENTED_EDGE('',*,*,#5489,.T.);
#7079=ORIENTED_EDGE('',*,*,#5491,.T.);
#7080=ORIENTED_EDGE('',*,*,#5508,.T.);
#7081=ORIENTED_EDGE('',*,*,#5509,.F.);
#7082=ORIENTED_EDGE('',*,*,#5478,.F.);
#7083=ORIENTED_EDGE('',*,*,#5498,.F.);
#7084=ORIENTED_EDGE('',*,*,#5463,.T.);
#7085=ORIENTED_EDGE('',*,*,#5480,.T.);
#7086=ORIENTED_EDGE('',*,*,#5510,.F.);
#7087=ORIENTED_EDGE('',*,*,#5511,.F.);
#7088=ORIENTED_EDGE('',*,*,#5499,.F.);
#7089=ORIENTED_EDGE('',*,*,#5481,.T.);
#7090=ORIENTED_EDGE('',*,*,#5465,.T.);
#7091=ORIENTED_EDGE('',*,*,#5467,.T.);
#7092=ORIENTED_EDGE('',*,*,#5486,.T.);
#7093=ORIENTED_EDGE('',*,*,#5511,.T.);
#7094=ORIENTED_EDGE('',*,*,#5512,.F.);
#7095=ORIENTED_EDGE('',*,*,#5513,.F.);
#7096=ORIENTED_EDGE('',*,*,#5500,.F.);
#7097=ORIENTED_EDGE('',*,*,#5513,.T.);
#7098=ORIENTED_EDGE('',*,*,#5514,.F.);
#7099=ORIENTED_EDGE('',*,*,#5515,.F.);
#7100=ORIENTED_EDGE('',*,*,#5501,.F.);
#7101=ORIENTED_EDGE('',*,*,#5484,.T.);
#7102=ORIENTED_EDGE('',*,*,#5515,.T.);
#7103=ORIENTED_EDGE('',*,*,#5516,.F.);
#7104=ORIENTED_EDGE('',*,*,#5517,.F.);
#7105=ORIENTED_EDGE('',*,*,#5502,.F.);
#7106=ORIENTED_EDGE('',*,*,#5517,.T.);
#7107=ORIENTED_EDGE('',*,*,#5518,.F.);
#7108=ORIENTED_EDGE('',*,*,#5519,.F.);
#7109=ORIENTED_EDGE('',*,*,#5503,.F.);
#7110=ORIENTED_EDGE('',*,*,#5488,.T.);
#7111=ORIENTED_EDGE('',*,*,#5519,.T.);
#7112=ORIENTED_EDGE('',*,*,#5520,.F.);
#7113=ORIENTED_EDGE('',*,*,#5475,.F.);
#7114=ORIENTED_EDGE('',*,*,#5504,.F.);
#7115=ORIENTED_EDGE('',*,*,#5469,.T.);
#7116=ORIENTED_EDGE('',*,*,#5476,.T.);
#7117=ORIENTED_EDGE('',*,*,#5520,.T.);
#7118=ORIENTED_EDGE('',*,*,#5518,.T.);
#7119=ORIENTED_EDGE('',*,*,#5516,.T.);
#7120=ORIENTED_EDGE('',*,*,#5514,.T.);
#7121=ORIENTED_EDGE('',*,*,#5512,.T.);
#7122=ORIENTED_EDGE('',*,*,#5510,.T.);
#7123=ORIENTED_EDGE('',*,*,#5479,.T.);
#7124=ORIENTED_EDGE('',*,*,#5509,.T.);
#7125=ORIENTED_EDGE('',*,*,#5507,.T.);
#7126=ORIENTED_EDGE('',*,*,#5505,.T.);
#7127=ORIENTED_EDGE('',*,*,#5495,.T.);
#7128=ORIENTED_EDGE('',*,*,#5521,.T.);
#7129=ORIENTED_EDGE('',*,*,#5522,.T.);
#7130=ORIENTED_EDGE('',*,*,#5523,.T.);
#7131=ORIENTED_EDGE('',*,*,#5522,.F.);
#7132=ORIENTED_EDGE('',*,*,#5523,.F.);
#7133=ORIENTED_EDGE('',*,*,#5524,.T.);
#7134=ORIENTED_EDGE('',*,*,#5525,.T.);
#7135=ORIENTED_EDGE('',*,*,#5524,.F.);
#7136=ORIENTED_EDGE('',*,*,#5526,.T.);
#7137=ORIENTED_EDGE('',*,*,#5521,.F.);
#7138=ORIENTED_EDGE('',*,*,#5526,.F.);
#7139=ORIENTED_EDGE('',*,*,#5527,.T.);
#7140=ORIENTED_EDGE('',*,*,#5528,.T.);
#7141=ORIENTED_EDGE('',*,*,#5527,.F.);
#7142=ORIENTED_EDGE('',*,*,#5528,.F.);
#7143=ORIENTED_EDGE('',*,*,#5525,.F.);
#7144=ORIENTED_EDGE('',*,*,#5529,.T.);
#7145=ORIENTED_EDGE('',*,*,#5530,.T.);
#7146=ORIENTED_EDGE('',*,*,#5531,.T.);
#7147=ORIENTED_EDGE('',*,*,#5532,.F.);
#7148=ORIENTED_EDGE('',*,*,#5533,.T.);
#7149=ORIENTED_EDGE('',*,*,#5534,.T.);
#7150=ORIENTED_EDGE('',*,*,#5535,.T.);
#7151=ORIENTED_EDGE('',*,*,#5530,.F.);
#7152=ORIENTED_EDGE('',*,*,#5536,.T.);
#7153=ORIENTED_EDGE('',*,*,#5537,.T.);
#7154=ORIENTED_EDGE('',*,*,#5538,.T.);
#7155=ORIENTED_EDGE('',*,*,#5534,.F.);
#7156=ORIENTED_EDGE('',*,*,#5539,.T.);
#7157=ORIENTED_EDGE('',*,*,#5540,.T.);
#7158=ORIENTED_EDGE('',*,*,#5541,.T.);
#7159=ORIENTED_EDGE('',*,*,#5537,.F.);
#7160=ORIENTED_EDGE('',*,*,#5542,.T.);
#7161=ORIENTED_EDGE('',*,*,#5543,.T.);
#7162=ORIENTED_EDGE('',*,*,#5544,.T.);
#7163=ORIENTED_EDGE('',*,*,#5540,.F.);
#7164=ORIENTED_EDGE('',*,*,#5545,.T.);
#7165=ORIENTED_EDGE('',*,*,#5532,.T.);
#7166=ORIENTED_EDGE('',*,*,#5546,.T.);
#7167=ORIENTED_EDGE('',*,*,#5543,.F.);
#7168=ORIENTED_EDGE('',*,*,#5545,.F.);
#7169=ORIENTED_EDGE('',*,*,#5542,.F.);
#7170=ORIENTED_EDGE('',*,*,#5539,.F.);
#7171=ORIENTED_EDGE('',*,*,#5536,.F.);
#7172=ORIENTED_EDGE('',*,*,#5533,.F.);
#7173=ORIENTED_EDGE('',*,*,#5529,.F.);
#7174=ORIENTED_EDGE('',*,*,#5546,.F.);
#7175=ORIENTED_EDGE('',*,*,#5531,.F.);
#7176=ORIENTED_EDGE('',*,*,#5535,.F.);
#7177=ORIENTED_EDGE('',*,*,#5538,.F.);
#7178=ORIENTED_EDGE('',*,*,#5541,.F.);
#7179=ORIENTED_EDGE('',*,*,#5544,.F.);
#7180=ORIENTED_EDGE('',*,*,#5547,.F.);
#7181=ORIENTED_EDGE('',*,*,#5548,.F.);
#7182=ORIENTED_EDGE('',*,*,#5549,.F.);
#7183=ORIENTED_EDGE('',*,*,#5550,.T.);
#7184=ORIENTED_EDGE('',*,*,#5548,.T.);
#7185=ORIENTED_EDGE('',*,*,#5550,.F.);
#7186=ORIENTED_EDGE('',*,*,#5551,.F.);
#7187=ORIENTED_EDGE('',*,*,#5552,.T.);
#7188=ORIENTED_EDGE('',*,*,#5549,.T.);
#7189=ORIENTED_EDGE('',*,*,#5552,.F.);
#7190=ORIENTED_EDGE('',*,*,#5553,.F.);
#7191=ORIENTED_EDGE('',*,*,#5554,.T.);
#7192=ORIENTED_EDGE('',*,*,#5551,.T.);
#7193=ORIENTED_EDGE('',*,*,#5554,.F.);
#7194=ORIENTED_EDGE('',*,*,#5553,.T.);
#7195=ORIENTED_EDGE('',*,*,#5555,.F.);
#7196=ORIENTED_EDGE('',*,*,#5556,.F.);
#7197=ORIENTED_EDGE('',*,*,#5557,.T.);
#7198=ORIENTED_EDGE('',*,*,#5555,.T.);
#7199=ORIENTED_EDGE('',*,*,#5557,.F.);
#7200=ORIENTED_EDGE('',*,*,#5547,.T.);
#7201=ORIENTED_EDGE('',*,*,#5558,.T.);
#7202=ORIENTED_EDGE('',*,*,#5556,.T.);
#7203=ORIENTED_EDGE('',*,*,#5558,.F.);
#7204=ORIENTED_EDGE('',*,*,#5559,.F.);
#7205=ORIENTED_EDGE('',*,*,#5560,.F.);
#7206=ORIENTED_EDGE('',*,*,#5561,.T.);
#7207=ORIENTED_EDGE('',*,*,#5559,.T.);
#7208=ORIENTED_EDGE('',*,*,#5561,.F.);
#7209=ORIENTED_EDGE('',*,*,#5562,.F.);
#7210=ORIENTED_EDGE('',*,*,#5563,.T.);
#7211=ORIENTED_EDGE('',*,*,#5560,.T.);
#7212=ORIENTED_EDGE('',*,*,#5563,.F.);
#7213=ORIENTED_EDGE('',*,*,#5564,.F.);
#7214=ORIENTED_EDGE('',*,*,#5565,.T.);
#7215=ORIENTED_EDGE('',*,*,#5562,.T.);
#7216=ORIENTED_EDGE('',*,*,#5565,.F.);
#7217=ORIENTED_EDGE('',*,*,#5564,.T.);
#7218=ORIENTED_EDGE('',*,*,#5566,.F.);
#7219=ORIENTED_EDGE('',*,*,#5567,.F.);
#7220=ORIENTED_EDGE('',*,*,#5568,.T.);
#7221=ORIENTED_EDGE('',*,*,#5566,.T.);
#7222=ORIENTED_EDGE('',*,*,#5568,.F.);
#7223=ORIENTED_EDGE('',*,*,#5569,.F.);
#7224=ORIENTED_EDGE('',*,*,#5570,.T.);
#7225=ORIENTED_EDGE('',*,*,#5567,.T.);
#7226=ORIENTED_EDGE('',*,*,#5570,.F.);
#7227=ORIENTED_EDGE('',*,*,#5571,.F.);
#7228=ORIENTED_EDGE('',*,*,#5572,.T.);
#7229=ORIENTED_EDGE('',*,*,#5569,.T.);
#7230=ORIENTED_EDGE('',*,*,#5572,.F.);
#7231=ORIENTED_EDGE('',*,*,#5571,.T.);
#7232=ORIENTED_EDGE('',*,*,#5573,.T.);
#7233=ORIENTED_EDGE('',*,*,#5574,.T.);
#7234=ORIENTED_EDGE('',*,*,#5575,.T.);
#7235=ORIENTED_EDGE('',*,*,#5576,.F.);
#7236=ORIENTED_EDGE('',*,*,#5577,.T.);
#7237=ORIENTED_EDGE('',*,*,#5578,.T.);
#7238=ORIENTED_EDGE('',*,*,#5579,.T.);
#7239=ORIENTED_EDGE('',*,*,#5574,.F.);
#7240=ORIENTED_EDGE('',*,*,#5580,.T.);
#7241=ORIENTED_EDGE('',*,*,#5581,.T.);
#7242=ORIENTED_EDGE('',*,*,#5582,.T.);
#7243=ORIENTED_EDGE('',*,*,#5578,.F.);
#7244=ORIENTED_EDGE('',*,*,#5583,.T.);
#7245=ORIENTED_EDGE('',*,*,#5584,.T.);
#7246=ORIENTED_EDGE('',*,*,#5585,.T.);
#7247=ORIENTED_EDGE('',*,*,#5581,.F.);
#7248=ORIENTED_EDGE('',*,*,#5586,.T.);
#7249=ORIENTED_EDGE('',*,*,#5587,.T.);
#7250=ORIENTED_EDGE('',*,*,#5588,.T.);
#7251=ORIENTED_EDGE('',*,*,#5584,.F.);
#7252=ORIENTED_EDGE('',*,*,#5589,.T.);
#7253=ORIENTED_EDGE('',*,*,#5576,.T.);
#7254=ORIENTED_EDGE('',*,*,#5590,.T.);
#7255=ORIENTED_EDGE('',*,*,#5587,.F.);
#7256=ORIENTED_EDGE('',*,*,#5589,.F.);
#7257=ORIENTED_EDGE('',*,*,#5586,.F.);
#7258=ORIENTED_EDGE('',*,*,#5583,.F.);
#7259=ORIENTED_EDGE('',*,*,#5580,.F.);
#7260=ORIENTED_EDGE('',*,*,#5577,.F.);
#7261=ORIENTED_EDGE('',*,*,#5573,.F.);
#7262=ORIENTED_EDGE('',*,*,#5590,.F.);
#7263=ORIENTED_EDGE('',*,*,#5575,.F.);
#7264=ORIENTED_EDGE('',*,*,#5579,.F.);
#7265=ORIENTED_EDGE('',*,*,#5582,.F.);
#7266=ORIENTED_EDGE('',*,*,#5585,.F.);
#7267=ORIENTED_EDGE('',*,*,#5588,.F.);
#7268=ORIENTED_EDGE('',*,*,#5591,.F.);
#7269=ORIENTED_EDGE('',*,*,#5592,.T.);
#7270=ORIENTED_EDGE('',*,*,#5593,.T.);
#7271=ORIENTED_EDGE('',*,*,#5594,.T.);
#7272=ORIENTED_EDGE('',*,*,#5593,.F.);
#7273=ORIENTED_EDGE('',*,*,#5591,.T.);
#7274=ORIENTED_EDGE('',*,*,#5595,.T.);
#7275=ORIENTED_EDGE('',*,*,#5592,.F.);
#7276=ORIENTED_EDGE('',*,*,#5595,.F.);
#7277=ORIENTED_EDGE('',*,*,#5594,.F.);
#7278=ORIENTED_EDGE('',*,*,#5596,.F.);
#7279=ORIENTED_EDGE('',*,*,#5597,.F.);
#7280=ORIENTED_EDGE('',*,*,#5598,.F.);
#7281=ORIENTED_EDGE('',*,*,#5599,.T.);
#7282=ORIENTED_EDGE('',*,*,#5600,.F.);
#7283=ORIENTED_EDGE('',*,*,#5599,.F.);
#7284=ORIENTED_EDGE('',*,*,#5601,.F.);
#7285=ORIENTED_EDGE('',*,*,#5602,.F.);
#7286=ORIENTED_EDGE('',*,*,#5603,.F.);
#7287=ORIENTED_EDGE('',*,*,#5602,.T.);
#7288=ORIENTED_EDGE('',*,*,#5604,.T.);
#7289=ORIENTED_EDGE('',*,*,#5605,.F.);
#7290=ORIENTED_EDGE('',*,*,#5601,.T.);
#7291=ORIENTED_EDGE('',*,*,#5598,.T.);
#7292=ORIENTED_EDGE('',*,*,#5606,.F.);
#7293=ORIENTED_EDGE('',*,*,#5604,.F.);
#7294=ORIENTED_EDGE('',*,*,#5596,.T.);
#7295=ORIENTED_EDGE('',*,*,#5600,.T.);
#7296=ORIENTED_EDGE('',*,*,#5603,.T.);
#7297=ORIENTED_EDGE('',*,*,#5607,.F.);
#7298=ORIENTED_EDGE('',*,*,#5608,.T.);
#7299=ORIENTED_EDGE('',*,*,#5609,.T.);
#7300=ORIENTED_EDGE('',*,*,#5608,.F.);
#7301=ORIENTED_EDGE('',*,*,#5610,.F.);
#7302=ORIENTED_EDGE('',*,*,#5597,.T.);
#7303=ORIENTED_EDGE('',*,*,#5610,.T.);
#7304=ORIENTED_EDGE('',*,*,#5607,.T.);
#7305=ORIENTED_EDGE('',*,*,#5605,.T.);
#7306=ORIENTED_EDGE('',*,*,#5606,.T.);
#7307=ORIENTED_EDGE('',*,*,#5609,.F.);
#7308=ORIENTED_EDGE('',*,*,#5611,.F.);
#7309=ORIENTED_EDGE('',*,*,#5612,.T.);
#7310=ORIENTED_EDGE('',*,*,#5613,.F.);
#7311=ORIENTED_EDGE('',*,*,#5614,.F.);
#7312=ORIENTED_EDGE('',*,*,#5615,.T.);
#7313=ORIENTED_EDGE('',*,*,#5616,.F.);
#7314=ORIENTED_EDGE('',*,*,#5617,.F.);
#7315=ORIENTED_EDGE('',*,*,#5615,.F.);
#7316=ORIENTED_EDGE('',*,*,#5618,.F.);
#7317=ORIENTED_EDGE('',*,*,#5619,.F.);
#7318=ORIENTED_EDGE('',*,*,#5612,.F.);
#7319=ORIENTED_EDGE('',*,*,#5620,.F.);
#7320=ORIENTED_EDGE('',*,*,#5618,.T.);
#7321=ORIENTED_EDGE('',*,*,#5614,.T.);
#7322=ORIENTED_EDGE('',*,*,#5621,.F.);
#7323=ORIENTED_EDGE('',*,*,#5622,.T.);
#7324=ORIENTED_EDGE('',*,*,#5623,.T.);
#7325=ORIENTED_EDGE('',*,*,#5622,.F.);
#7326=ORIENTED_EDGE('',*,*,#5619,.T.);
#7327=ORIENTED_EDGE('',*,*,#5620,.T.);
#7328=ORIENTED_EDGE('',*,*,#5613,.T.);
#7329=ORIENTED_EDGE('',*,*,#5611,.T.);
#7330=ORIENTED_EDGE('',*,*,#5624,.F.);
#7331=ORIENTED_EDGE('',*,*,#5625,.T.);
#7332=ORIENTED_EDGE('',*,*,#5626,.T.);
#7333=ORIENTED_EDGE('',*,*,#5625,.F.);
#7334=ORIENTED_EDGE('',*,*,#5616,.T.);
#7335=ORIENTED_EDGE('',*,*,#5617,.T.);
#7336=ORIENTED_EDGE('',*,*,#5624,.T.);
#7337=ORIENTED_EDGE('',*,*,#5621,.T.);
#7338=ORIENTED_EDGE('',*,*,#5626,.F.);
#7339=ORIENTED_EDGE('',*,*,#5623,.F.);
#7340=ORIENTED_EDGE('',*,*,#5627,.F.);
#7341=ORIENTED_EDGE('',*,*,#5628,.T.);
#7342=ORIENTED_EDGE('',*,*,#5629,.F.);
#7343=ORIENTED_EDGE('',*,*,#5630,.F.);
#7344=ORIENTED_EDGE('',*,*,#5631,.T.);
#7345=ORIENTED_EDGE('',*,*,#5632,.F.);
#7346=ORIENTED_EDGE('',*,*,#5633,.F.);
#7347=ORIENTED_EDGE('',*,*,#5631,.F.);
#7348=ORIENTED_EDGE('',*,*,#5634,.F.);
#7349=ORIENTED_EDGE('',*,*,#5635,.F.);
#7350=ORIENTED_EDGE('',*,*,#5628,.F.);
#7351=ORIENTED_EDGE('',*,*,#5636,.F.);
#7352=ORIENTED_EDGE('',*,*,#5634,.T.);
#7353=ORIENTED_EDGE('',*,*,#5630,.T.);
#7354=ORIENTED_EDGE('',*,*,#5637,.F.);
#7355=ORIENTED_EDGE('',*,*,#5638,.T.);
#7356=ORIENTED_EDGE('',*,*,#5639,.T.);
#7357=ORIENTED_EDGE('',*,*,#5638,.F.);
#7358=ORIENTED_EDGE('',*,*,#5635,.T.);
#7359=ORIENTED_EDGE('',*,*,#5636,.T.);
#7360=ORIENTED_EDGE('',*,*,#5629,.T.);
#7361=ORIENTED_EDGE('',*,*,#5627,.T.);
#7362=ORIENTED_EDGE('',*,*,#5640,.F.);
#7363=ORIENTED_EDGE('',*,*,#5641,.T.);
#7364=ORIENTED_EDGE('',*,*,#5642,.T.);
#7365=ORIENTED_EDGE('',*,*,#5641,.F.);
#7366=ORIENTED_EDGE('',*,*,#5632,.T.);
#7367=ORIENTED_EDGE('',*,*,#5633,.T.);
#7368=ORIENTED_EDGE('',*,*,#5640,.T.);
#7369=ORIENTED_EDGE('',*,*,#5637,.T.);
#7370=ORIENTED_EDGE('',*,*,#5642,.F.);
#7371=ORIENTED_EDGE('',*,*,#5639,.F.);
#7372=ORIENTED_EDGE('',*,*,#5643,.F.);
#7373=ORIENTED_EDGE('',*,*,#5644,.T.);
#7374=ORIENTED_EDGE('',*,*,#5645,.T.);
#7375=ORIENTED_EDGE('',*,*,#5644,.F.);
#7376=ORIENTED_EDGE('',*,*,#5646,.F.);
#7377=ORIENTED_EDGE('',*,*,#5647,.T.);
#7378=ORIENTED_EDGE('',*,*,#5648,.T.);
#7379=ORIENTED_EDGE('',*,*,#5647,.F.);
#7380=ORIENTED_EDGE('',*,*,#5646,.T.);
#7381=ORIENTED_EDGE('',*,*,#5643,.T.);
#7382=ORIENTED_EDGE('',*,*,#5648,.F.);
#7383=ORIENTED_EDGE('',*,*,#5645,.F.);
#7384=ORIENTED_EDGE('',*,*,#5649,.F.);
#7385=ORIENTED_EDGE('',*,*,#5650,.F.);
#7386=ORIENTED_EDGE('',*,*,#5651,.F.);
#7387=ORIENTED_EDGE('',*,*,#5652,.F.);
#7388=ORIENTED_EDGE('',*,*,#5652,.T.);
#7389=ORIENTED_EDGE('',*,*,#5653,.T.);
#7390=ORIENTED_EDGE('',*,*,#5654,.T.);
#7391=ORIENTED_EDGE('',*,*,#5655,.T.);
#7392=ORIENTED_EDGE('',*,*,#5656,.T.);
#7393=ORIENTED_EDGE('',*,*,#5657,.T.);
#7394=ORIENTED_EDGE('',*,*,#5658,.F.);
#7395=ORIENTED_EDGE('',*,*,#5659,.T.);
#7396=ORIENTED_EDGE('',*,*,#5660,.F.);
#7397=ORIENTED_EDGE('',*,*,#5659,.F.);
#7398=ORIENTED_EDGE('',*,*,#5658,.T.);
#7399=ORIENTED_EDGE('',*,*,#5661,.F.);
#7400=ORIENTED_EDGE('',*,*,#5662,.T.);
#7401=ORIENTED_EDGE('',*,*,#5663,.F.);
#7402=ORIENTED_EDGE('',*,*,#5664,.F.);
#7403=ORIENTED_EDGE('',*,*,#5665,.F.);
#7404=ORIENTED_EDGE('',*,*,#5666,.F.);
#7405=ORIENTED_EDGE('',*,*,#5667,.F.);
#7406=ORIENTED_EDGE('',*,*,#5668,.F.);
#7407=ORIENTED_EDGE('',*,*,#5669,.F.);
#7408=ORIENTED_EDGE('',*,*,#5662,.F.);
#7409=ORIENTED_EDGE('',*,*,#5670,.F.);
#7410=ORIENTED_EDGE('',*,*,#5664,.T.);
#7411=ORIENTED_EDGE('',*,*,#5665,.T.);
#7412=ORIENTED_EDGE('',*,*,#5670,.T.);
#7413=ORIENTED_EDGE('',*,*,#5663,.T.);
#7414=ORIENTED_EDGE('',*,*,#5661,.T.);
#7415=ORIENTED_EDGE('',*,*,#5669,.T.);
#7416=ORIENTED_EDGE('',*,*,#5671,.T.);
#7417=ORIENTED_EDGE('',*,*,#5672,.T.);
#7418=ORIENTED_EDGE('',*,*,#5657,.F.);
#7419=ORIENTED_EDGE('',*,*,#5673,.T.);
#7420=ORIENTED_EDGE('',*,*,#5674,.T.);
#7421=ORIENTED_EDGE('',*,*,#5675,.F.);
#7422=ORIENTED_EDGE('',*,*,#5676,.T.);
#7423=ORIENTED_EDGE('',*,*,#5654,.F.);
#7424=ORIENTED_EDGE('',*,*,#5672,.F.);
#7425=ORIENTED_EDGE('',*,*,#5677,.F.);
#7426=ORIENTED_EDGE('',*,*,#5678,.T.);
#7427=ORIENTED_EDGE('',*,*,#5655,.F.);
#7428=ORIENTED_EDGE('',*,*,#5676,.F.);
#7429=ORIENTED_EDGE('',*,*,#5679,.F.);
#7430=ORIENTED_EDGE('',*,*,#5673,.F.);
#7431=ORIENTED_EDGE('',*,*,#5656,.F.);
#7432=ORIENTED_EDGE('',*,*,#5678,.F.);
#7433=ORIENTED_EDGE('',*,*,#5680,.T.);
#7434=ORIENTED_EDGE('',*,*,#5660,.T.);
#7435=ORIENTED_EDGE('',*,*,#5681,.F.);
#7436=ORIENTED_EDGE('',*,*,#5650,.T.);
#7437=ORIENTED_EDGE('',*,*,#5682,.F.);
#7438=ORIENTED_EDGE('',*,*,#5683,.F.);
#7439=ORIENTED_EDGE('',*,*,#5680,.F.);
#7440=ORIENTED_EDGE('',*,*,#5684,.T.);
#7441=ORIENTED_EDGE('',*,*,#5682,.T.);
#7442=ORIENTED_EDGE('',*,*,#5684,.F.);
#7443=ORIENTED_EDGE('',*,*,#5683,.T.);
#7444=ORIENTED_EDGE('',*,*,#5685,.T.);
#7445=ORIENTED_EDGE('',*,*,#5686,.T.);
#7446=ORIENTED_EDGE('',*,*,#5667,.T.);
#7447=ORIENTED_EDGE('',*,*,#5687,.T.);
#7448=ORIENTED_EDGE('',*,*,#5685,.F.);
#7449=ORIENTED_EDGE('',*,*,#5649,.T.);
#7450=ORIENTED_EDGE('',*,*,#5653,.F.);
#7451=ORIENTED_EDGE('',*,*,#5651,.T.);
#7452=ORIENTED_EDGE('',*,*,#5681,.T.);
#7453=ORIENTED_EDGE('',*,*,#5666,.T.);
#7454=ORIENTED_EDGE('',*,*,#5674,.F.);
#7455=ORIENTED_EDGE('',*,*,#5679,.T.);
#7456=ORIENTED_EDGE('',*,*,#5677,.T.);
#7457=ORIENTED_EDGE('',*,*,#5675,.T.);
#7458=ORIENTED_EDGE('',*,*,#5671,.F.);
#7459=ORIENTED_EDGE('',*,*,#5668,.T.);
#7460=ORIENTED_EDGE('',*,*,#5686,.F.);
#7461=ORIENTED_EDGE('',*,*,#5687,.F.);
#7462=ORIENTED_EDGE('',*,*,#5688,.F.);
#7463=ORIENTED_EDGE('',*,*,#5689,.T.);
#7464=ORIENTED_EDGE('',*,*,#5690,.F.);
#7465=ORIENTED_EDGE('',*,*,#5689,.F.);
#7466=ORIENTED_EDGE('',*,*,#5688,.T.);
#7467=ORIENTED_EDGE('',*,*,#5691,.F.);
#7468=ORIENTED_EDGE('',*,*,#5692,.T.);
#7469=ORIENTED_EDGE('',*,*,#5693,.F.);
#7470=ORIENTED_EDGE('',*,*,#5694,.T.);
#7471=ORIENTED_EDGE('',*,*,#5691,.T.);
#7472=ORIENTED_EDGE('',*,*,#5694,.F.);
#7473=ORIENTED_EDGE('',*,*,#5693,.T.);
#7474=ORIENTED_EDGE('',*,*,#5690,.T.);
#7475=ORIENTED_EDGE('',*,*,#5692,.F.);
#7476=ORIENTED_EDGE('',*,*,#5695,.T.);
#7477=ORIENTED_EDGE('',*,*,#5696,.T.);
#7478=ORIENTED_EDGE('',*,*,#5695,.F.);
#7479=ORIENTED_EDGE('',*,*,#5696,.F.);
#7480=ORIENTED_EDGE('',*,*,#5697,.F.);
#7481=ORIENTED_EDGE('',*,*,#5698,.T.);
#7482=ORIENTED_EDGE('',*,*,#5699,.T.);
#7483=ORIENTED_EDGE('',*,*,#5698,.F.);
#7484=ORIENTED_EDGE('',*,*,#5700,.F.);
#7485=ORIENTED_EDGE('',*,*,#5701,.T.);
#7486=ORIENTED_EDGE('',*,*,#5702,.T.);
#7487=ORIENTED_EDGE('',*,*,#5701,.F.);
#7488=ORIENTED_EDGE('',*,*,#5700,.T.);
#7489=ORIENTED_EDGE('',*,*,#5697,.T.);
#7490=ORIENTED_EDGE('',*,*,#5702,.F.);
#7491=ORIENTED_EDGE('',*,*,#5699,.F.);
#7492=ORIENTED_EDGE('',*,*,#5703,.F.);
#7493=ORIENTED_EDGE('',*,*,#5704,.T.);
#7494=ORIENTED_EDGE('',*,*,#5705,.T.);
#7495=ORIENTED_EDGE('',*,*,#5704,.F.);
#7496=ORIENTED_EDGE('',*,*,#5706,.F.);
#7497=ORIENTED_EDGE('',*,*,#5707,.T.);
#7498=ORIENTED_EDGE('',*,*,#5708,.T.);
#7499=ORIENTED_EDGE('',*,*,#5707,.F.);
#7500=ORIENTED_EDGE('',*,*,#5706,.T.);
#7501=ORIENTED_EDGE('',*,*,#5703,.T.);
#7502=ORIENTED_EDGE('',*,*,#5708,.F.);
#7503=ORIENTED_EDGE('',*,*,#5705,.F.);
#7504=ORIENTED_EDGE('',*,*,#5709,.F.);
#7505=ORIENTED_EDGE('',*,*,#5710,.T.);
#7506=ORIENTED_EDGE('',*,*,#5711,.T.);
#7507=ORIENTED_EDGE('',*,*,#5710,.F.);
#7508=ORIENTED_EDGE('',*,*,#5712,.F.);
#7509=ORIENTED_EDGE('',*,*,#5713,.T.);
#7510=ORIENTED_EDGE('',*,*,#5714,.T.);
#7511=ORIENTED_EDGE('',*,*,#5713,.F.);
#7512=ORIENTED_EDGE('',*,*,#5712,.T.);
#7513=ORIENTED_EDGE('',*,*,#5709,.T.);
#7514=ORIENTED_EDGE('',*,*,#5714,.F.);
#7515=ORIENTED_EDGE('',*,*,#5711,.F.);
#7516=ORIENTED_EDGE('',*,*,#5715,.F.);
#7517=ORIENTED_EDGE('',*,*,#5716,.F.);
#7518=ORIENTED_EDGE('',*,*,#5717,.F.);
#7519=ORIENTED_EDGE('',*,*,#5718,.F.);
#7520=ORIENTED_EDGE('',*,*,#5719,.F.);
#7521=ORIENTED_EDGE('',*,*,#5720,.F.);
#7522=ORIENTED_EDGE('',*,*,#5721,.F.);
#7523=ORIENTED_EDGE('',*,*,#5722,.F.);
#7524=ORIENTED_EDGE('',*,*,#5719,.T.);
#7525=ORIENTED_EDGE('',*,*,#5723,.T.);
#7526=ORIENTED_EDGE('',*,*,#5724,.T.);
#7527=ORIENTED_EDGE('',*,*,#5725,.T.);
#7528=ORIENTED_EDGE('',*,*,#5718,.T.);
#7529=ORIENTED_EDGE('',*,*,#5726,.F.);
#7530=ORIENTED_EDGE('',*,*,#5727,.T.);
#7531=ORIENTED_EDGE('',*,*,#5723,.F.);
#7532=ORIENTED_EDGE('',*,*,#5717,.T.);
#7533=ORIENTED_EDGE('',*,*,#5728,.T.);
#7534=ORIENTED_EDGE('',*,*,#5729,.T.);
#7535=ORIENTED_EDGE('',*,*,#5726,.T.);
#7536=ORIENTED_EDGE('',*,*,#5716,.T.);
#7537=ORIENTED_EDGE('',*,*,#5730,.F.);
#7538=ORIENTED_EDGE('',*,*,#5731,.T.);
#7539=ORIENTED_EDGE('',*,*,#5728,.F.);
#7540=ORIENTED_EDGE('',*,*,#5732,.F.);
#7541=ORIENTED_EDGE('',*,*,#5733,.F.);
#7542=ORIENTED_EDGE('',*,*,#5724,.F.);
#7543=ORIENTED_EDGE('',*,*,#5727,.F.);
#7544=ORIENTED_EDGE('',*,*,#5729,.F.);
#7545=ORIENTED_EDGE('',*,*,#5731,.F.);
#7546=ORIENTED_EDGE('',*,*,#5734,.F.);
#7547=ORIENTED_EDGE('',*,*,#5735,.F.);
#7548=ORIENTED_EDGE('',*,*,#5720,.T.);
#7549=ORIENTED_EDGE('',*,*,#5725,.F.);
#7550=ORIENTED_EDGE('',*,*,#5733,.T.);
#7551=ORIENTED_EDGE('',*,*,#5736,.F.);
#7552=ORIENTED_EDGE('',*,*,#5715,.T.);
#7553=ORIENTED_EDGE('',*,*,#5737,.T.);
#7554=ORIENTED_EDGE('',*,*,#5734,.T.);
#7555=ORIENTED_EDGE('',*,*,#5730,.T.);
#7556=ORIENTED_EDGE('',*,*,#5721,.T.);
#7557=ORIENTED_EDGE('',*,*,#5736,.T.);
#7558=ORIENTED_EDGE('',*,*,#5732,.T.);
#7559=ORIENTED_EDGE('',*,*,#5738,.T.);
#7560=ORIENTED_EDGE('',*,*,#5722,.T.);
#7561=ORIENTED_EDGE('',*,*,#5738,.F.);
#7562=ORIENTED_EDGE('',*,*,#5735,.T.);
#7563=ORIENTED_EDGE('',*,*,#5737,.F.);
#7564=ORIENTED_EDGE('',*,*,#5739,.F.);
#7565=ORIENTED_EDGE('',*,*,#5740,.T.);
#7566=ORIENTED_EDGE('',*,*,#5741,.T.);
#7567=ORIENTED_EDGE('',*,*,#5742,.F.);
#7568=ORIENTED_EDGE('',*,*,#5743,.F.);
#7569=ORIENTED_EDGE('',*,*,#5744,.T.);
#7570=ORIENTED_EDGE('',*,*,#5745,.T.);
#7571=ORIENTED_EDGE('',*,*,#5740,.F.);
#7572=ORIENTED_EDGE('',*,*,#5746,.F.);
#7573=ORIENTED_EDGE('',*,*,#5747,.T.);
#7574=ORIENTED_EDGE('',*,*,#5748,.T.);
#7575=ORIENTED_EDGE('',*,*,#5744,.F.);
#7576=ORIENTED_EDGE('',*,*,#5749,.F.);
#7577=ORIENTED_EDGE('',*,*,#5750,.T.);
#7578=ORIENTED_EDGE('',*,*,#5751,.T.);
#7579=ORIENTED_EDGE('',*,*,#5747,.F.);
#7580=ORIENTED_EDGE('',*,*,#5752,.F.);
#7581=ORIENTED_EDGE('',*,*,#5753,.T.);
#7582=ORIENTED_EDGE('',*,*,#5754,.T.);
#7583=ORIENTED_EDGE('',*,*,#5750,.F.);
#7584=ORIENTED_EDGE('',*,*,#5755,.F.);
#7585=ORIENTED_EDGE('',*,*,#5742,.T.);
#7586=ORIENTED_EDGE('',*,*,#5756,.T.);
#7587=ORIENTED_EDGE('',*,*,#5753,.F.);
#7588=ORIENTED_EDGE('',*,*,#5756,.F.);
#7589=ORIENTED_EDGE('',*,*,#5741,.F.);
#7590=ORIENTED_EDGE('',*,*,#5745,.F.);
#7591=ORIENTED_EDGE('',*,*,#5748,.F.);
#7592=ORIENTED_EDGE('',*,*,#5751,.F.);
#7593=ORIENTED_EDGE('',*,*,#5754,.F.);
#7594=ORIENTED_EDGE('',*,*,#5757,.F.);
#7595=ORIENTED_EDGE('',*,*,#5739,.T.);
#7596=ORIENTED_EDGE('',*,*,#5755,.T.);
#7597=ORIENTED_EDGE('',*,*,#5752,.T.);
#7598=ORIENTED_EDGE('',*,*,#5749,.T.);
#7599=ORIENTED_EDGE('',*,*,#5746,.T.);
#7600=ORIENTED_EDGE('',*,*,#5743,.T.);
#7601=ORIENTED_EDGE('',*,*,#5758,.F.);
#7602=ORIENTED_EDGE('',*,*,#5759,.T.);
#7603=ORIENTED_EDGE('',*,*,#5757,.T.);
#7604=ORIENTED_EDGE('',*,*,#5759,.F.);
#7605=ORIENTED_EDGE('',*,*,#5760,.F.);
#7606=ORIENTED_EDGE('',*,*,#5761,.T.);
#7607=ORIENTED_EDGE('',*,*,#5758,.T.);
#7608=ORIENTED_EDGE('',*,*,#5761,.F.);
#7609=ORIENTED_EDGE('',*,*,#5762,.F.);
#7610=ORIENTED_EDGE('',*,*,#5763,.T.);
#7611=ORIENTED_EDGE('',*,*,#5760,.T.);
#7612=ORIENTED_EDGE('',*,*,#5763,.F.);
#7613=ORIENTED_EDGE('',*,*,#5762,.T.);
#7614=ORIENTED_EDGE('',*,*,#5764,.F.);
#7615=ORIENTED_EDGE('',*,*,#5765,.T.);
#7616=ORIENTED_EDGE('',*,*,#5766,.F.);
#7617=ORIENTED_EDGE('',*,*,#5765,.F.);
#7618=ORIENTED_EDGE('',*,*,#5767,.F.);
#7619=ORIENTED_EDGE('',*,*,#5768,.T.);
#7620=ORIENTED_EDGE('',*,*,#5769,.F.);
#7621=ORIENTED_EDGE('',*,*,#5768,.F.);
#7622=ORIENTED_EDGE('',*,*,#5770,.F.);
#7623=ORIENTED_EDGE('',*,*,#5771,.T.);
#7624=ORIENTED_EDGE('',*,*,#5772,.F.);
#7625=ORIENTED_EDGE('',*,*,#5773,.F.);
#7626=ORIENTED_EDGE('',*,*,#5773,.T.);
#7627=ORIENTED_EDGE('',*,*,#5774,.T.);
#7628=ORIENTED_EDGE('',*,*,#5775,.T.);
#7629=ORIENTED_EDGE('',*,*,#5776,.T.);
#7630=ORIENTED_EDGE('',*,*,#5766,.T.);
#7631=ORIENTED_EDGE('',*,*,#5769,.T.);
#7632=ORIENTED_EDGE('',*,*,#5772,.T.);
#7633=ORIENTED_EDGE('',*,*,#5777,.F.);
#7634=ORIENTED_EDGE('',*,*,#5778,.T.);
#7635=ORIENTED_EDGE('',*,*,#5774,.F.);
#7636=ORIENTED_EDGE('',*,*,#5779,.F.);
#7637=ORIENTED_EDGE('',*,*,#5775,.F.);
#7638=ORIENTED_EDGE('',*,*,#5778,.F.);
#7639=ORIENTED_EDGE('',*,*,#5780,.T.);
#7640=ORIENTED_EDGE('',*,*,#5770,.T.);
#7641=ORIENTED_EDGE('',*,*,#5776,.F.);
#7642=ORIENTED_EDGE('',*,*,#5779,.T.);
#7643=ORIENTED_EDGE('',*,*,#5781,.F.);
#7644=ORIENTED_EDGE('',*,*,#5781,.T.);
#7645=ORIENTED_EDGE('',*,*,#5780,.F.);
#7646=ORIENTED_EDGE('',*,*,#5777,.T.);
#7647=ORIENTED_EDGE('',*,*,#5771,.F.);
#7648=ORIENTED_EDGE('',*,*,#5764,.T.);
#7649=ORIENTED_EDGE('',*,*,#5767,.T.);
#7650=ORIENTED_EDGE('',*,*,#5782,.F.);
#7651=ORIENTED_EDGE('',*,*,#5783,.T.);
#7652=ORIENTED_EDGE('',*,*,#5784,.T.);
#7653=ORIENTED_EDGE('',*,*,#5783,.F.);
#7654=ORIENTED_EDGE('',*,*,#5785,.F.);
#7655=ORIENTED_EDGE('',*,*,#5786,.T.);
#7656=ORIENTED_EDGE('',*,*,#5787,.T.);
#7657=ORIENTED_EDGE('',*,*,#5786,.F.);
#7658=ORIENTED_EDGE('',*,*,#5785,.T.);
#7659=ORIENTED_EDGE('',*,*,#5782,.T.);
#7660=ORIENTED_EDGE('',*,*,#5787,.F.);
#7661=ORIENTED_EDGE('',*,*,#5784,.F.);
#7662=ORIENTED_EDGE('',*,*,#5788,.F.);
#7663=ORIENTED_EDGE('',*,*,#5789,.T.);
#7664=ORIENTED_EDGE('',*,*,#5790,.T.);
#7665=ORIENTED_EDGE('',*,*,#5789,.F.);
#7666=ORIENTED_EDGE('',*,*,#5791,.F.);
#7667=ORIENTED_EDGE('',*,*,#5792,.T.);
#7668=ORIENTED_EDGE('',*,*,#5793,.T.);
#7669=ORIENTED_EDGE('',*,*,#5792,.F.);
#7670=ORIENTED_EDGE('',*,*,#5791,.T.);
#7671=ORIENTED_EDGE('',*,*,#5788,.T.);
#7672=ORIENTED_EDGE('',*,*,#5793,.F.);
#7673=ORIENTED_EDGE('',*,*,#5790,.F.);
#7674=ORIENTED_EDGE('',*,*,#5794,.F.);
#7675=ORIENTED_EDGE('',*,*,#5795,.T.);
#7676=ORIENTED_EDGE('',*,*,#5796,.T.);
#7677=ORIENTED_EDGE('',*,*,#5795,.F.);
#7678=ORIENTED_EDGE('',*,*,#5797,.F.);
#7679=ORIENTED_EDGE('',*,*,#5798,.T.);
#7680=ORIENTED_EDGE('',*,*,#5799,.T.);
#7681=ORIENTED_EDGE('',*,*,#5798,.F.);
#7682=ORIENTED_EDGE('',*,*,#5797,.T.);
#7683=ORIENTED_EDGE('',*,*,#5794,.T.);
#7684=ORIENTED_EDGE('',*,*,#5799,.F.);
#7685=ORIENTED_EDGE('',*,*,#5796,.F.);
#7686=ORIENTED_EDGE('',*,*,#5800,.F.);
#7687=ORIENTED_EDGE('',*,*,#5801,.T.);
#7688=ORIENTED_EDGE('',*,*,#5802,.T.);
#7689=ORIENTED_EDGE('',*,*,#5801,.F.);
#7690=ORIENTED_EDGE('',*,*,#5803,.F.);
#7691=ORIENTED_EDGE('',*,*,#5804,.T.);
#7692=ORIENTED_EDGE('',*,*,#5805,.T.);
#7693=ORIENTED_EDGE('',*,*,#5804,.F.);
#7694=ORIENTED_EDGE('',*,*,#5803,.T.);
#7695=ORIENTED_EDGE('',*,*,#5800,.T.);
#7696=ORIENTED_EDGE('',*,*,#5805,.F.);
#7697=ORIENTED_EDGE('',*,*,#5802,.F.);
#7698=ORIENTED_EDGE('',*,*,#5806,.F.);
#7699=ORIENTED_EDGE('',*,*,#5807,.F.);
#7700=ORIENTED_EDGE('',*,*,#5808,.T.);
#7701=ORIENTED_EDGE('',*,*,#5809,.F.);
#7702=ORIENTED_EDGE('',*,*,#5810,.F.);
#7703=ORIENTED_EDGE('',*,*,#5808,.F.);
#7704=ORIENTED_EDGE('',*,*,#5809,.T.);
#7705=ORIENTED_EDGE('',*,*,#5810,.T.);
#7706=ORIENTED_EDGE('',*,*,#5811,.T.);
#7707=ORIENTED_EDGE('',*,*,#5812,.T.);
#7708=ORIENTED_EDGE('',*,*,#5811,.F.);
#7709=ORIENTED_EDGE('',*,*,#5813,.T.);
#7710=ORIENTED_EDGE('',*,*,#5814,.T.);
#7711=ORIENTED_EDGE('',*,*,#5815,.F.);
#7712=ORIENTED_EDGE('',*,*,#5814,.F.);
#7713=ORIENTED_EDGE('',*,*,#5815,.T.);
#7714=ORIENTED_EDGE('',*,*,#5816,.T.);
#7715=ORIENTED_EDGE('',*,*,#5817,.F.);
#7716=ORIENTED_EDGE('',*,*,#5816,.F.);
#7717=ORIENTED_EDGE('',*,*,#5812,.F.);
#7718=ORIENTED_EDGE('',*,*,#5817,.T.);
#7719=ORIENTED_EDGE('',*,*,#5818,.F.);
#7720=ORIENTED_EDGE('',*,*,#5819,.T.);
#7721=ORIENTED_EDGE('',*,*,#5806,.T.);
#7722=ORIENTED_EDGE('',*,*,#5807,.T.);
#7723=ORIENTED_EDGE('',*,*,#5819,.F.);
#7724=ORIENTED_EDGE('',*,*,#5818,.T.);
#7725=ORIENTED_EDGE('',*,*,#5820,.F.);
#7726=ORIENTED_EDGE('',*,*,#5820,.T.);
#7727=ORIENTED_EDGE('',*,*,#5821,.T.);
#7728=ORIENTED_EDGE('',*,*,#5813,.F.);
#7729=ORIENTED_EDGE('',*,*,#5821,.F.);
#7730=ORIENTED_EDGE('',*,*,#5822,.F.);
#7731=ORIENTED_EDGE('',*,*,#5823,.F.);
#7732=ORIENTED_EDGE('',*,*,#5824,.T.);
#7733=ORIENTED_EDGE('',*,*,#5825,.F.);
#7734=ORIENTED_EDGE('',*,*,#5826,.F.);
#7735=ORIENTED_EDGE('',*,*,#5824,.F.);
#7736=ORIENTED_EDGE('',*,*,#5827,.T.);
#7737=ORIENTED_EDGE('',*,*,#5828,.T.);
#7738=ORIENTED_EDGE('',*,*,#5825,.T.);
#7739=ORIENTED_EDGE('',*,*,#5826,.T.);
#7740=ORIENTED_EDGE('',*,*,#5828,.F.);
#7741=ORIENTED_EDGE('',*,*,#5829,.F.);
#7742=ORIENTED_EDGE('',*,*,#5830,.T.);
#7743=ORIENTED_EDGE('',*,*,#5831,.F.);
#7744=ORIENTED_EDGE('',*,*,#5832,.T.);
#7745=ORIENTED_EDGE('',*,*,#5829,.T.);
#7746=ORIENTED_EDGE('',*,*,#5832,.F.);
#7747=ORIENTED_EDGE('',*,*,#5833,.F.);
#7748=ORIENTED_EDGE('',*,*,#5834,.T.);
#7749=ORIENTED_EDGE('',*,*,#5831,.T.);
#7750=ORIENTED_EDGE('',*,*,#5834,.F.);
#7751=ORIENTED_EDGE('',*,*,#5835,.F.);
#7752=ORIENTED_EDGE('',*,*,#5836,.T.);
#7753=ORIENTED_EDGE('',*,*,#5833,.T.);
#7754=ORIENTED_EDGE('',*,*,#5836,.F.);
#7755=ORIENTED_EDGE('',*,*,#5835,.T.);
#7756=ORIENTED_EDGE('',*,*,#5827,.F.);
#7757=ORIENTED_EDGE('',*,*,#5822,.T.);
#7758=ORIENTED_EDGE('',*,*,#5823,.T.);
#7759=ORIENTED_EDGE('',*,*,#5837,.T.);
#7760=ORIENTED_EDGE('',*,*,#5830,.F.);
#7761=ORIENTED_EDGE('',*,*,#5837,.F.);
#7762=ORIENTED_EDGE('',*,*,#5838,.T.);
#7763=ORIENTED_EDGE('',*,*,#5838,.F.);
#7764=ORIENTED_EDGE('',*,*,#5839,.T.);
#7765=ORIENTED_EDGE('',*,*,#5839,.F.);
#7766=ORIENTED_EDGE('',*,*,#5840,.T.);
#7767=ORIENTED_EDGE('',*,*,#5840,.F.);
#7768=ORIENTED_EDGE('',*,*,#5841,.T.);
#7769=ORIENTED_EDGE('',*,*,#5841,.F.);
#7770=ORIENTED_EDGE('',*,*,#5842,.T.);
#7771=ORIENTED_EDGE('',*,*,#5842,.F.);
#7772=ORIENTED_EDGE('',*,*,#5843,.T.);
#7773=ORIENTED_EDGE('',*,*,#5843,.F.);
#7774=ORIENTED_EDGE('',*,*,#5844,.T.);
#7775=ORIENTED_EDGE('',*,*,#5844,.F.);
#7776=ORIENTED_EDGE('',*,*,#5845,.T.);
#7777=ORIENTED_EDGE('',*,*,#5845,.F.);
#7778=ORIENTED_EDGE('',*,*,#5846,.F.);
#7779=ORIENTED_EDGE('',*,*,#5847,.F.);
#7780=ORIENTED_EDGE('',*,*,#5848,.F.);
#7781=ORIENTED_EDGE('',*,*,#5849,.F.);
#7782=ORIENTED_EDGE('',*,*,#5848,.T.);
#7783=ORIENTED_EDGE('',*,*,#5850,.F.);
#7784=ORIENTED_EDGE('',*,*,#5851,.T.);
#7785=ORIENTED_EDGE('',*,*,#5852,.F.);
#7786=ORIENTED_EDGE('',*,*,#5853,.T.);
#7787=ORIENTED_EDGE('',*,*,#5854,.F.);
#7788=ORIENTED_EDGE('',*,*,#5855,.T.);
#7789=ORIENTED_EDGE('',*,*,#5856,.T.);
#7790=ORIENTED_EDGE('',*,*,#5857,.F.);
#7791=ORIENTED_EDGE('',*,*,#5856,.F.);
#7792=ORIENTED_EDGE('',*,*,#5858,.T.);
#7793=ORIENTED_EDGE('',*,*,#5859,.F.);
#7794=ORIENTED_EDGE('',*,*,#5860,.T.);
#7795=ORIENTED_EDGE('',*,*,#5861,.F.);
#7796=ORIENTED_EDGE('',*,*,#5862,.T.);
#7797=ORIENTED_EDGE('',*,*,#5863,.F.);
#7798=ORIENTED_EDGE('',*,*,#5864,.T.);
#7799=ORIENTED_EDGE('',*,*,#5865,.F.);
#7800=ORIENTED_EDGE('',*,*,#5866,.T.);
#7801=ORIENTED_EDGE('',*,*,#5867,.F.);
#7802=ORIENTED_EDGE('',*,*,#5847,.T.);
#7803=ORIENTED_EDGE('',*,*,#5868,.T.);
#7804=ORIENTED_EDGE('',*,*,#5869,.T.);
#7805=ORIENTED_EDGE('',*,*,#5850,.T.);
#7806=ORIENTED_EDGE('',*,*,#5870,.F.);
#7807=ORIENTED_EDGE('',*,*,#5871,.F.);
#7808=ORIENTED_EDGE('',*,*,#5851,.F.);
#7809=ORIENTED_EDGE('',*,*,#5869,.F.);
#7810=ORIENTED_EDGE('',*,*,#5871,.T.);
#7811=ORIENTED_EDGE('',*,*,#5872,.T.);
#7812=ORIENTED_EDGE('',*,*,#5873,.T.);
#7813=ORIENTED_EDGE('',*,*,#5852,.T.);
#7814=ORIENTED_EDGE('',*,*,#5874,.F.);
#7815=ORIENTED_EDGE('',*,*,#5875,.F.);
#7816=ORIENTED_EDGE('',*,*,#5853,.F.);
#7817=ORIENTED_EDGE('',*,*,#5873,.F.);
#7818=ORIENTED_EDGE('',*,*,#5875,.T.);
#7819=ORIENTED_EDGE('',*,*,#5876,.T.);
#7820=ORIENTED_EDGE('',*,*,#5877,.T.);
#7821=ORIENTED_EDGE('',*,*,#5854,.T.);
#7822=ORIENTED_EDGE('',*,*,#5878,.F.);
#7823=ORIENTED_EDGE('',*,*,#5879,.F.);
#7824=ORIENTED_EDGE('',*,*,#5858,.F.);
#7825=ORIENTED_EDGE('',*,*,#5855,.F.);
#7826=ORIENTED_EDGE('',*,*,#5877,.F.);
#7827=ORIENTED_EDGE('',*,*,#5880,.F.);
#7828=ORIENTED_EDGE('',*,*,#5879,.T.);
#7829=ORIENTED_EDGE('',*,*,#5881,.T.);
#7830=ORIENTED_EDGE('',*,*,#5882,.T.);
#7831=ORIENTED_EDGE('',*,*,#5859,.T.);
#7832=ORIENTED_EDGE('',*,*,#5883,.F.);
#7833=ORIENTED_EDGE('',*,*,#5884,.F.);
#7834=ORIENTED_EDGE('',*,*,#5860,.F.);
#7835=ORIENTED_EDGE('',*,*,#5882,.F.);
#7836=ORIENTED_EDGE('',*,*,#5884,.T.);
#7837=ORIENTED_EDGE('',*,*,#5885,.T.);
#7838=ORIENTED_EDGE('',*,*,#5886,.T.);
#7839=ORIENTED_EDGE('',*,*,#5861,.T.);
#7840=ORIENTED_EDGE('',*,*,#5887,.F.);
#7841=ORIENTED_EDGE('',*,*,#5888,.F.);
#7842=ORIENTED_EDGE('',*,*,#5862,.F.);
#7843=ORIENTED_EDGE('',*,*,#5886,.F.);
#7844=ORIENTED_EDGE('',*,*,#5888,.T.);
#7845=ORIENTED_EDGE('',*,*,#5889,.T.);
#7846=ORIENTED_EDGE('',*,*,#5890,.T.);
#7847=ORIENTED_EDGE('',*,*,#5863,.T.);
#7848=ORIENTED_EDGE('',*,*,#5864,.F.);
#7849=ORIENTED_EDGE('',*,*,#5890,.F.);
#7850=ORIENTED_EDGE('',*,*,#5891,.F.);
#7851=ORIENTED_EDGE('',*,*,#5892,.F.);
#7852=ORIENTED_EDGE('',*,*,#5893,.F.);
#7853=ORIENTED_EDGE('',*,*,#5894,.T.);
#7854=ORIENTED_EDGE('',*,*,#5880,.T.);
#7855=ORIENTED_EDGE('',*,*,#5876,.F.);
#7856=ORIENTED_EDGE('',*,*,#5874,.T.);
#7857=ORIENTED_EDGE('',*,*,#5872,.F.);
#7858=ORIENTED_EDGE('',*,*,#5870,.T.);
#7859=ORIENTED_EDGE('',*,*,#5868,.F.);
#7860=ORIENTED_EDGE('',*,*,#5846,.T.);
#7861=ORIENTED_EDGE('',*,*,#5895,.F.);
#7862=ORIENTED_EDGE('',*,*,#5896,.T.);
#7863=ORIENTED_EDGE('',*,*,#5897,.F.);
#7864=ORIENTED_EDGE('',*,*,#5891,.T.);
#7865=ORIENTED_EDGE('',*,*,#5889,.F.);
#7866=ORIENTED_EDGE('',*,*,#5887,.T.);
#7867=ORIENTED_EDGE('',*,*,#5885,.F.);
#7868=ORIENTED_EDGE('',*,*,#5883,.T.);
#7869=ORIENTED_EDGE('',*,*,#5881,.F.);
#7870=ORIENTED_EDGE('',*,*,#5878,.T.);
#7871=ORIENTED_EDGE('',*,*,#5894,.F.);
#7872=ORIENTED_EDGE('',*,*,#5849,.T.);
#7873=ORIENTED_EDGE('',*,*,#5867,.T.);
#7874=ORIENTED_EDGE('',*,*,#5898,.T.);
#7875=ORIENTED_EDGE('',*,*,#5895,.T.);
#7876=ORIENTED_EDGE('',*,*,#5866,.F.);
#7877=ORIENTED_EDGE('',*,*,#5899,.F.);
#7878=ORIENTED_EDGE('',*,*,#5896,.F.);
#7879=ORIENTED_EDGE('',*,*,#5898,.F.);
#7880=ORIENTED_EDGE('',*,*,#5857,.T.);
#7881=ORIENTED_EDGE('',*,*,#5893,.T.);
#7882=ORIENTED_EDGE('',*,*,#5892,.T.);
#7883=ORIENTED_EDGE('',*,*,#5897,.T.);
#7884=ORIENTED_EDGE('',*,*,#5899,.T.);
#7885=ORIENTED_EDGE('',*,*,#5865,.T.);
#7886=ORIENTED_EDGE('',*,*,#5900,.F.);
#7887=ORIENTED_EDGE('',*,*,#5901,.T.);
#7888=ORIENTED_EDGE('',*,*,#5902,.F.);
#7889=ORIENTED_EDGE('',*,*,#5903,.T.);
#7890=ORIENTED_EDGE('',*,*,#5900,.T.);
#7891=ORIENTED_EDGE('',*,*,#5903,.F.);
#7892=ORIENTED_EDGE('',*,*,#5902,.T.);
#7893=ORIENTED_EDGE('',*,*,#5904,.F.);
#7894=ORIENTED_EDGE('',*,*,#5904,.T.);
#7895=ORIENTED_EDGE('',*,*,#5905,.T.);
#7896=ORIENTED_EDGE('',*,*,#5901,.F.);
#7897=ORIENTED_EDGE('',*,*,#5905,.F.);
#7898=ORIENTED_EDGE('',*,*,#5906,.F.);
#7899=ORIENTED_EDGE('',*,*,#5907,.T.);
#7900=ORIENTED_EDGE('',*,*,#5908,.F.);
#7901=ORIENTED_EDGE('',*,*,#5909,.T.);
#7902=ORIENTED_EDGE('',*,*,#5906,.T.);
#7903=ORIENTED_EDGE('',*,*,#5909,.F.);
#7904=ORIENTED_EDGE('',*,*,#5908,.T.);
#7905=ORIENTED_EDGE('',*,*,#5910,.F.);
#7906=ORIENTED_EDGE('',*,*,#5910,.T.);
#7907=ORIENTED_EDGE('',*,*,#5911,.T.);
#7908=ORIENTED_EDGE('',*,*,#5907,.F.);
#7909=ORIENTED_EDGE('',*,*,#5911,.F.);
#7910=ORIENTED_EDGE('',*,*,#5912,.F.);
#7911=ORIENTED_EDGE('',*,*,#5913,.T.);
#7912=ORIENTED_EDGE('',*,*,#5914,.F.);
#7913=ORIENTED_EDGE('',*,*,#5913,.F.);
#7914=ORIENTED_EDGE('',*,*,#5915,.F.);
#7915=ORIENTED_EDGE('',*,*,#5916,.T.);
#7916=ORIENTED_EDGE('',*,*,#5917,.T.);
#7917=ORIENTED_EDGE('',*,*,#5918,.T.);
#7918=ORIENTED_EDGE('',*,*,#5912,.T.);
#7919=ORIENTED_EDGE('',*,*,#5919,.F.);
#7920=ORIENTED_EDGE('',*,*,#5920,.F.);
#7921=ORIENTED_EDGE('',*,*,#5921,.F.);
#7922=ORIENTED_EDGE('',*,*,#5916,.F.);
#7923=ORIENTED_EDGE('',*,*,#5922,.F.);
#7924=ORIENTED_EDGE('',*,*,#5918,.F.);
#7925=ORIENTED_EDGE('',*,*,#5923,.T.);
#7926=ORIENTED_EDGE('',*,*,#5924,.F.);
#7927=ORIENTED_EDGE('',*,*,#5917,.F.);
#7928=ORIENTED_EDGE('',*,*,#5921,.T.);
#7929=ORIENTED_EDGE('',*,*,#5925,.F.);
#7930=ORIENTED_EDGE('',*,*,#5923,.F.);
#7931=ORIENTED_EDGE('',*,*,#5926,.F.);
#7932=ORIENTED_EDGE('',*,*,#5924,.T.);
#7933=ORIENTED_EDGE('',*,*,#5925,.T.);
#7934=ORIENTED_EDGE('',*,*,#5920,.T.);
#7935=ORIENTED_EDGE('',*,*,#5914,.T.);
#7936=ORIENTED_EDGE('',*,*,#5927,.F.);
#7937=ORIENTED_EDGE('',*,*,#5928,.T.);
#7938=ORIENTED_EDGE('',*,*,#5929,.F.);
#7939=ORIENTED_EDGE('',*,*,#5928,.F.);
#7940=ORIENTED_EDGE('',*,*,#5930,.F.);
#7941=ORIENTED_EDGE('',*,*,#5931,.T.);
#7942=ORIENTED_EDGE('',*,*,#5932,.F.);
#7943=ORIENTED_EDGE('',*,*,#5931,.F.);
#7944=ORIENTED_EDGE('',*,*,#5933,.F.);
#7945=ORIENTED_EDGE('',*,*,#5934,.T.);
#7946=ORIENTED_EDGE('',*,*,#5935,.F.);
#7947=ORIENTED_EDGE('',*,*,#5934,.F.);
#7948=ORIENTED_EDGE('',*,*,#5936,.F.);
#7949=ORIENTED_EDGE('',*,*,#5937,.T.);
#7950=ORIENTED_EDGE('',*,*,#5938,.F.);
#7951=ORIENTED_EDGE('',*,*,#5937,.F.);
#7952=ORIENTED_EDGE('',*,*,#5939,.F.);
#7953=ORIENTED_EDGE('',*,*,#5940,.T.);
#7954=ORIENTED_EDGE('',*,*,#5941,.F.);
#7955=ORIENTED_EDGE('',*,*,#5940,.F.);
#7956=ORIENTED_EDGE('',*,*,#5942,.F.);
#7957=ORIENTED_EDGE('',*,*,#5943,.T.);
#7958=ORIENTED_EDGE('',*,*,#5944,.F.);
#7959=ORIENTED_EDGE('',*,*,#5943,.F.);
#7960=ORIENTED_EDGE('',*,*,#5945,.T.);
#7961=ORIENTED_EDGE('',*,*,#5946,.T.);
#7962=ORIENTED_EDGE('',*,*,#5947,.F.);
#7963=ORIENTED_EDGE('',*,*,#5948,.F.);
#7964=ORIENTED_EDGE('',*,*,#5949,.T.);
#7965=ORIENTED_EDGE('',*,*,#5948,.T.);
#7966=ORIENTED_EDGE('',*,*,#5950,.F.);
#7967=ORIENTED_EDGE('',*,*,#5951,.F.);
#7968=ORIENTED_EDGE('',*,*,#5944,.T.);
#7969=ORIENTED_EDGE('',*,*,#5941,.T.);
#7970=ORIENTED_EDGE('',*,*,#5938,.T.);
#7971=ORIENTED_EDGE('',*,*,#5935,.T.);
#7972=ORIENTED_EDGE('',*,*,#5932,.T.);
#7973=ORIENTED_EDGE('',*,*,#5929,.T.);
#7974=ORIENTED_EDGE('',*,*,#5952,.T.);
#7975=ORIENTED_EDGE('',*,*,#5951,.T.);
#7976=ORIENTED_EDGE('',*,*,#5953,.F.);
#7977=ORIENTED_EDGE('',*,*,#5954,.F.);
#7978=ORIENTED_EDGE('',*,*,#5955,.T.);
#7979=ORIENTED_EDGE('',*,*,#5954,.T.);
#7980=ORIENTED_EDGE('',*,*,#5956,.F.);
#7981=ORIENTED_EDGE('',*,*,#5946,.F.);
#7982=ORIENTED_EDGE('',*,*,#5942,.T.);
#7983=ORIENTED_EDGE('',*,*,#5939,.T.);
#7984=ORIENTED_EDGE('',*,*,#5936,.T.);
#7985=ORIENTED_EDGE('',*,*,#5933,.T.);
#7986=ORIENTED_EDGE('',*,*,#5930,.T.);
#7987=ORIENTED_EDGE('',*,*,#5927,.T.);
#7988=ORIENTED_EDGE('',*,*,#5956,.T.);
#7989=ORIENTED_EDGE('',*,*,#5953,.T.);
#7990=ORIENTED_EDGE('',*,*,#5950,.T.);
#7991=ORIENTED_EDGE('',*,*,#5947,.T.);
#7992=ORIENTED_EDGE('',*,*,#5919,.T.);
#7993=ORIENTED_EDGE('',*,*,#5915,.T.);
#7994=ORIENTED_EDGE('',*,*,#5922,.T.);
#7995=ORIENTED_EDGE('',*,*,#5926,.T.);
#7996=ORIENTED_EDGE('',*,*,#5955,.F.);
#7997=ORIENTED_EDGE('',*,*,#5945,.F.);
#7998=ORIENTED_EDGE('',*,*,#5949,.F.);
#7999=ORIENTED_EDGE('',*,*,#5952,.F.);
#8000=ORIENTED_EDGE('',*,*,#5957,.F.);
#8001=ORIENTED_EDGE('',*,*,#5958,.T.);
#8002=ORIENTED_EDGE('',*,*,#5959,.F.);
#8003=ORIENTED_EDGE('',*,*,#5958,.F.);
#8004=ORIENTED_EDGE('',*,*,#5960,.F.);
#8005=ORIENTED_EDGE('',*,*,#5961,.T.);
#8006=ORIENTED_EDGE('',*,*,#5962,.F.);
#8007=ORIENTED_EDGE('',*,*,#5961,.F.);
#8008=ORIENTED_EDGE('',*,*,#5963,.F.);
#8009=ORIENTED_EDGE('',*,*,#5964,.T.);
#8010=ORIENTED_EDGE('',*,*,#5965,.F.);
#8011=ORIENTED_EDGE('',*,*,#5964,.F.);
#8012=ORIENTED_EDGE('',*,*,#5966,.F.);
#8013=ORIENTED_EDGE('',*,*,#5967,.T.);
#8014=ORIENTED_EDGE('',*,*,#5968,.F.);
#8015=ORIENTED_EDGE('',*,*,#5967,.F.);
#8016=ORIENTED_EDGE('',*,*,#5969,.F.);
#8017=ORIENTED_EDGE('',*,*,#5970,.T.);
#8018=ORIENTED_EDGE('',*,*,#5971,.F.);
#8019=ORIENTED_EDGE('',*,*,#5970,.F.);
#8020=ORIENTED_EDGE('',*,*,#5972,.F.);
#8021=ORIENTED_EDGE('',*,*,#5973,.T.);
#8022=ORIENTED_EDGE('',*,*,#5974,.F.);
#8023=ORIENTED_EDGE('',*,*,#5973,.F.);
#8024=ORIENTED_EDGE('',*,*,#5975,.T.);
#8025=ORIENTED_EDGE('',*,*,#5976,.T.);
#8026=ORIENTED_EDGE('',*,*,#5977,.F.);
#8027=ORIENTED_EDGE('',*,*,#5978,.F.);
#8028=ORIENTED_EDGE('',*,*,#5979,.T.);
#8029=ORIENTED_EDGE('',*,*,#5978,.T.);
#8030=ORIENTED_EDGE('',*,*,#5980,.F.);
#8031=ORIENTED_EDGE('',*,*,#5981,.F.);
#8032=ORIENTED_EDGE('',*,*,#5974,.T.);
#8033=ORIENTED_EDGE('',*,*,#5971,.T.);
#8034=ORIENTED_EDGE('',*,*,#5968,.T.);
#8035=ORIENTED_EDGE('',*,*,#5965,.T.);
#8036=ORIENTED_EDGE('',*,*,#5962,.T.);
#8037=ORIENTED_EDGE('',*,*,#5959,.T.);
#8038=ORIENTED_EDGE('',*,*,#5982,.T.);
#8039=ORIENTED_EDGE('',*,*,#5981,.T.);
#8040=ORIENTED_EDGE('',*,*,#5983,.F.);
#8041=ORIENTED_EDGE('',*,*,#5984,.F.);
#8042=ORIENTED_EDGE('',*,*,#5985,.T.);
#8043=ORIENTED_EDGE('',*,*,#5984,.T.);
#8044=ORIENTED_EDGE('',*,*,#5986,.F.);
#8045=ORIENTED_EDGE('',*,*,#5976,.F.);
#8046=ORIENTED_EDGE('',*,*,#5972,.T.);
#8047=ORIENTED_EDGE('',*,*,#5969,.T.);
#8048=ORIENTED_EDGE('',*,*,#5966,.T.);
#8049=ORIENTED_EDGE('',*,*,#5963,.T.);
#8050=ORIENTED_EDGE('',*,*,#5960,.T.);
#8051=ORIENTED_EDGE('',*,*,#5957,.T.);
#8052=ORIENTED_EDGE('',*,*,#5986,.T.);
#8053=ORIENTED_EDGE('',*,*,#5983,.T.);
#8054=ORIENTED_EDGE('',*,*,#5980,.T.);
#8055=ORIENTED_EDGE('',*,*,#5977,.T.);
#8056=ORIENTED_EDGE('',*,*,#5985,.F.);
#8057=ORIENTED_EDGE('',*,*,#5975,.F.);
#8058=ORIENTED_EDGE('',*,*,#5979,.F.);
#8059=ORIENTED_EDGE('',*,*,#5982,.F.);
#8060=ORIENTED_EDGE('',*,*,#5987,.F.);
#8061=ORIENTED_EDGE('',*,*,#5988,.T.);
#8062=ORIENTED_EDGE('',*,*,#5989,.F.);
#8063=ORIENTED_EDGE('',*,*,#5988,.F.);
#8064=ORIENTED_EDGE('',*,*,#5990,.F.);
#8065=ORIENTED_EDGE('',*,*,#5991,.T.);
#8066=ORIENTED_EDGE('',*,*,#5992,.F.);
#8067=ORIENTED_EDGE('',*,*,#5991,.F.);
#8068=ORIENTED_EDGE('',*,*,#5993,.F.);
#8069=ORIENTED_EDGE('',*,*,#5994,.T.);
#8070=ORIENTED_EDGE('',*,*,#5995,.F.);
#8071=ORIENTED_EDGE('',*,*,#5994,.F.);
#8072=ORIENTED_EDGE('',*,*,#5996,.F.);
#8073=ORIENTED_EDGE('',*,*,#5997,.T.);
#8074=ORIENTED_EDGE('',*,*,#5998,.F.);
#8075=ORIENTED_EDGE('',*,*,#5997,.F.);
#8076=ORIENTED_EDGE('',*,*,#5999,.F.);
#8077=ORIENTED_EDGE('',*,*,#6000,.T.);
#8078=ORIENTED_EDGE('',*,*,#6001,.F.);
#8079=ORIENTED_EDGE('',*,*,#6000,.F.);
#8080=ORIENTED_EDGE('',*,*,#6002,.F.);
#8081=ORIENTED_EDGE('',*,*,#6003,.T.);
#8082=ORIENTED_EDGE('',*,*,#6004,.F.);
#8083=ORIENTED_EDGE('',*,*,#6003,.F.);
#8084=ORIENTED_EDGE('',*,*,#6005,.T.);
#8085=ORIENTED_EDGE('',*,*,#6006,.T.);
#8086=ORIENTED_EDGE('',*,*,#6007,.F.);
#8087=ORIENTED_EDGE('',*,*,#6008,.F.);
#8088=ORIENTED_EDGE('',*,*,#6009,.T.);
#8089=ORIENTED_EDGE('',*,*,#6008,.T.);
#8090=ORIENTED_EDGE('',*,*,#6010,.F.);
#8091=ORIENTED_EDGE('',*,*,#6011,.F.);
#8092=ORIENTED_EDGE('',*,*,#6004,.T.);
#8093=ORIENTED_EDGE('',*,*,#6001,.T.);
#8094=ORIENTED_EDGE('',*,*,#5998,.T.);
#8095=ORIENTED_EDGE('',*,*,#5995,.T.);
#8096=ORIENTED_EDGE('',*,*,#5992,.T.);
#8097=ORIENTED_EDGE('',*,*,#5989,.T.);
#8098=ORIENTED_EDGE('',*,*,#6012,.T.);
#8099=ORIENTED_EDGE('',*,*,#6011,.T.);
#8100=ORIENTED_EDGE('',*,*,#6013,.F.);
#8101=ORIENTED_EDGE('',*,*,#6014,.F.);
#8102=ORIENTED_EDGE('',*,*,#6015,.T.);
#8103=ORIENTED_EDGE('',*,*,#6014,.T.);
#8104=ORIENTED_EDGE('',*,*,#6016,.F.);
#8105=ORIENTED_EDGE('',*,*,#6006,.F.);
#8106=ORIENTED_EDGE('',*,*,#6002,.T.);
#8107=ORIENTED_EDGE('',*,*,#5999,.T.);
#8108=ORIENTED_EDGE('',*,*,#5996,.T.);
#8109=ORIENTED_EDGE('',*,*,#5993,.T.);
#8110=ORIENTED_EDGE('',*,*,#5990,.T.);
#8111=ORIENTED_EDGE('',*,*,#5987,.T.);
#8112=ORIENTED_EDGE('',*,*,#6016,.T.);
#8113=ORIENTED_EDGE('',*,*,#6013,.T.);
#8114=ORIENTED_EDGE('',*,*,#6010,.T.);
#8115=ORIENTED_EDGE('',*,*,#6007,.T.);
#8116=ORIENTED_EDGE('',*,*,#6015,.F.);
#8117=ORIENTED_EDGE('',*,*,#6005,.F.);
#8118=ORIENTED_EDGE('',*,*,#6009,.F.);
#8119=ORIENTED_EDGE('',*,*,#6012,.F.);
#8120=ORIENTED_EDGE('',*,*,#6017,.F.);
#8121=ORIENTED_EDGE('',*,*,#6018,.T.);
#8122=ORIENTED_EDGE('',*,*,#6019,.F.);
#8123=ORIENTED_EDGE('',*,*,#6018,.F.);
#8124=ORIENTED_EDGE('',*,*,#6017,.T.);
#8125=ORIENTED_EDGE('',*,*,#6020,.T.);
#8126=ORIENTED_EDGE('',*,*,#6021,.F.);
#8127=ORIENTED_EDGE('',*,*,#6020,.F.);
#8128=ORIENTED_EDGE('',*,*,#6022,.T.);
#8129=ORIENTED_EDGE('',*,*,#6023,.T.);
#8130=ORIENTED_EDGE('',*,*,#6022,.F.);
#8131=ORIENTED_EDGE('',*,*,#6023,.F.);
#8132=ORIENTED_EDGE('',*,*,#6024,.F.);
#8133=ORIENTED_EDGE('',*,*,#6025,.T.);
#8134=ORIENTED_EDGE('',*,*,#6021,.T.);
#8135=ORIENTED_EDGE('',*,*,#6025,.F.);
#8136=ORIENTED_EDGE('',*,*,#6024,.T.);
#8137=ORIENTED_EDGE('',*,*,#6019,.T.);
#8138=ORIENTED_EDGE('',*,*,#6026,.F.);
#8139=ORIENTED_EDGE('',*,*,#6027,.T.);
#8140=ORIENTED_EDGE('',*,*,#6028,.T.);
#8141=ORIENTED_EDGE('',*,*,#6027,.F.);
#8142=ORIENTED_EDGE('',*,*,#6029,.F.);
#8143=ORIENTED_EDGE('',*,*,#6030,.T.);
#8144=ORIENTED_EDGE('',*,*,#6031,.T.);
#8145=ORIENTED_EDGE('',*,*,#6030,.F.);
#8146=ORIENTED_EDGE('',*,*,#6029,.T.);
#8147=ORIENTED_EDGE('',*,*,#6026,.T.);
#8148=ORIENTED_EDGE('',*,*,#6031,.F.);
#8149=ORIENTED_EDGE('',*,*,#6028,.F.);
#8150=ORIENTED_EDGE('',*,*,#6032,.F.);
#8151=ORIENTED_EDGE('',*,*,#6033,.T.);
#8152=ORIENTED_EDGE('',*,*,#6034,.T.);
#8153=ORIENTED_EDGE('',*,*,#6033,.F.);
#8154=ORIENTED_EDGE('',*,*,#6035,.F.);
#8155=ORIENTED_EDGE('',*,*,#6036,.T.);
#8156=ORIENTED_EDGE('',*,*,#6037,.T.);
#8157=ORIENTED_EDGE('',*,*,#6036,.F.);
#8158=ORIENTED_EDGE('',*,*,#6035,.T.);
#8159=ORIENTED_EDGE('',*,*,#6032,.T.);
#8160=ORIENTED_EDGE('',*,*,#6037,.F.);
#8161=ORIENTED_EDGE('',*,*,#6034,.F.);
#8162=ORIENTED_EDGE('',*,*,#6038,.F.);
#8163=ORIENTED_EDGE('',*,*,#6039,.T.);
#8164=ORIENTED_EDGE('',*,*,#6040,.T.);
#8165=ORIENTED_EDGE('',*,*,#6039,.F.);
#8166=ORIENTED_EDGE('',*,*,#6041,.F.);
#8167=ORIENTED_EDGE('',*,*,#6042,.T.);
#8168=ORIENTED_EDGE('',*,*,#6043,.T.);
#8169=ORIENTED_EDGE('',*,*,#6042,.F.);
#8170=ORIENTED_EDGE('',*,*,#6041,.T.);
#8171=ORIENTED_EDGE('',*,*,#6038,.T.);
#8172=ORIENTED_EDGE('',*,*,#6043,.F.);
#8173=ORIENTED_EDGE('',*,*,#6040,.F.);
#8174=ORIENTED_EDGE('',*,*,#6044,.F.);
#8175=ORIENTED_EDGE('',*,*,#6045,.F.);
#8176=ORIENTED_EDGE('',*,*,#6046,.F.);
#8177=ORIENTED_EDGE('',*,*,#6047,.F.);
#8178=ORIENTED_EDGE('',*,*,#6048,.F.);
#8179=ORIENTED_EDGE('',*,*,#6047,.T.);
#8180=ORIENTED_EDGE('',*,*,#6049,.F.);
#8181=ORIENTED_EDGE('',*,*,#6050,.T.);
#8182=ORIENTED_EDGE('',*,*,#6051,.F.);
#8183=ORIENTED_EDGE('',*,*,#6050,.F.);
#8184=ORIENTED_EDGE('',*,*,#6052,.F.);
#8185=ORIENTED_EDGE('',*,*,#6053,.F.);
#8186=ORIENTED_EDGE('',*,*,#6054,.F.);
#8187=ORIENTED_EDGE('',*,*,#6053,.T.);
#8188=ORIENTED_EDGE('',*,*,#6055,.T.);
#8189=ORIENTED_EDGE('',*,*,#6045,.T.);
#8190=ORIENTED_EDGE('',*,*,#6055,.F.);
#8191=ORIENTED_EDGE('',*,*,#6052,.T.);
#8192=ORIENTED_EDGE('',*,*,#6049,.T.);
#8193=ORIENTED_EDGE('',*,*,#6046,.T.);
#8194=ORIENTED_EDGE('',*,*,#6056,.F.);
#8195=ORIENTED_EDGE('',*,*,#6057,.T.);
#8196=ORIENTED_EDGE('',*,*,#6058,.F.);
#8197=ORIENTED_EDGE('',*,*,#6059,.T.);
#8198=ORIENTED_EDGE('',*,*,#6056,.T.);
#8199=ORIENTED_EDGE('',*,*,#6059,.F.);
#8200=ORIENTED_EDGE('',*,*,#6058,.T.);
#8201=ORIENTED_EDGE('',*,*,#6060,.F.);
#8202=ORIENTED_EDGE('',*,*,#6061,.F.);
#8203=ORIENTED_EDGE('',*,*,#6062,.T.);
#8204=ORIENTED_EDGE('',*,*,#6060,.T.);
#8205=ORIENTED_EDGE('',*,*,#6062,.F.);
#8206=ORIENTED_EDGE('',*,*,#6063,.F.);
#8207=ORIENTED_EDGE('',*,*,#6061,.T.);
#8208=ORIENTED_EDGE('',*,*,#6064,.F.);
#8209=ORIENTED_EDGE('',*,*,#6065,.T.);
#8210=ORIENTED_EDGE('',*,*,#6063,.T.);
#8211=ORIENTED_EDGE('',*,*,#6065,.F.);
#8212=ORIENTED_EDGE('',*,*,#6064,.T.);
#8213=ORIENTED_EDGE('',*,*,#6066,.F.);
#8214=ORIENTED_EDGE('',*,*,#6067,.F.);
#8215=ORIENTED_EDGE('',*,*,#6068,.T.);
#8216=ORIENTED_EDGE('',*,*,#6066,.T.);
#8217=ORIENTED_EDGE('',*,*,#6068,.F.);
#8218=ORIENTED_EDGE('',*,*,#6069,.F.);
#8219=ORIENTED_EDGE('',*,*,#6067,.T.);
#8220=ORIENTED_EDGE('',*,*,#6070,.F.);
#8221=ORIENTED_EDGE('',*,*,#6071,.T.);
#8222=ORIENTED_EDGE('',*,*,#6069,.T.);
#8223=ORIENTED_EDGE('',*,*,#6071,.F.);
#8224=ORIENTED_EDGE('',*,*,#6070,.T.);
#8225=ORIENTED_EDGE('',*,*,#6072,.F.);
#8226=ORIENTED_EDGE('',*,*,#6072,.T.);
#8227=ORIENTED_EDGE('',*,*,#6073,.T.);
#8228=ORIENTED_EDGE('',*,*,#6057,.F.);
#8229=ORIENTED_EDGE('',*,*,#6073,.F.);
#8230=ORIENTED_EDGE('',*,*,#6051,.T.);
#8231=ORIENTED_EDGE('',*,*,#6054,.T.);
#8232=ORIENTED_EDGE('',*,*,#6044,.T.);
#8233=ORIENTED_EDGE('',*,*,#6048,.T.);
#8234=ORIENTED_EDGE('',*,*,#6074,.F.);
#8235=ORIENTED_EDGE('',*,*,#6075,.F.);
#8236=ORIENTED_EDGE('',*,*,#6076,.F.);
#8237=ORIENTED_EDGE('',*,*,#6077,.F.);
#8238=ORIENTED_EDGE('',*,*,#6078,.F.);
#8239=ORIENTED_EDGE('',*,*,#6077,.T.);
#8240=ORIENTED_EDGE('',*,*,#6079,.F.);
#8241=ORIENTED_EDGE('',*,*,#6080,.T.);
#8242=ORIENTED_EDGE('',*,*,#6081,.F.);
#8243=ORIENTED_EDGE('',*,*,#6080,.F.);
#8244=ORIENTED_EDGE('',*,*,#6082,.F.);
#8245=ORIENTED_EDGE('',*,*,#6083,.F.);
#8246=ORIENTED_EDGE('',*,*,#6084,.F.);
#8247=ORIENTED_EDGE('',*,*,#6083,.T.);
#8248=ORIENTED_EDGE('',*,*,#6085,.F.);
#8249=ORIENTED_EDGE('',*,*,#6075,.T.);
#8250=ORIENTED_EDGE('',*,*,#6086,.F.);
#8251=ORIENTED_EDGE('',*,*,#6087,.T.);
#8252=ORIENTED_EDGE('',*,*,#6088,.F.);
#8253=ORIENTED_EDGE('',*,*,#6089,.T.);
#8254=ORIENTED_EDGE('',*,*,#6086,.T.);
#8255=ORIENTED_EDGE('',*,*,#6089,.F.);
#8256=ORIENTED_EDGE('',*,*,#6081,.T.);
#8257=ORIENTED_EDGE('',*,*,#6084,.T.);
#8258=ORIENTED_EDGE('',*,*,#6074,.T.);
#8259=ORIENTED_EDGE('',*,*,#6078,.T.);
#8260=ORIENTED_EDGE('',*,*,#6088,.T.);
#8261=ORIENTED_EDGE('',*,*,#6090,.F.);
#8262=ORIENTED_EDGE('',*,*,#6090,.T.);
#8263=ORIENTED_EDGE('',*,*,#6091,.T.);
#8264=ORIENTED_EDGE('',*,*,#6087,.F.);
#8265=ORIENTED_EDGE('',*,*,#6091,.F.);
#8266=ORIENTED_EDGE('',*,*,#6082,.T.);
#8267=ORIENTED_EDGE('',*,*,#6079,.T.);
#8268=ORIENTED_EDGE('',*,*,#6076,.T.);
#8269=ORIENTED_EDGE('',*,*,#6085,.T.);
#8270=ORIENTED_EDGE('',*,*,#6092,.T.);
#8271=ORIENTED_EDGE('',*,*,#6093,.T.);
#8272=ORIENTED_EDGE('',*,*,#6094,.T.);
#8273=ORIENTED_EDGE('',*,*,#6095,.F.);
#8274=ORIENTED_EDGE('',*,*,#6096,.T.);
#8275=ORIENTED_EDGE('',*,*,#6097,.T.);
#8276=ORIENTED_EDGE('',*,*,#6098,.T.);
#8277=ORIENTED_EDGE('',*,*,#6093,.F.);
#8278=ORIENTED_EDGE('',*,*,#6099,.T.);
#8279=ORIENTED_EDGE('',*,*,#6100,.T.);
#8280=ORIENTED_EDGE('',*,*,#6101,.T.);
#8281=ORIENTED_EDGE('',*,*,#6097,.F.);
#8282=ORIENTED_EDGE('',*,*,#6102,.T.);
#8283=ORIENTED_EDGE('',*,*,#6103,.T.);
#8284=ORIENTED_EDGE('',*,*,#6104,.T.);
#8285=ORIENTED_EDGE('',*,*,#6100,.F.);
#8286=ORIENTED_EDGE('',*,*,#6105,.T.);
#8287=ORIENTED_EDGE('',*,*,#6106,.T.);
#8288=ORIENTED_EDGE('',*,*,#6107,.T.);
#8289=ORIENTED_EDGE('',*,*,#6103,.F.);
#8290=ORIENTED_EDGE('',*,*,#6108,.T.);
#8291=ORIENTED_EDGE('',*,*,#6095,.T.);
#8292=ORIENTED_EDGE('',*,*,#6109,.T.);
#8293=ORIENTED_EDGE('',*,*,#6106,.F.);
#8294=ORIENTED_EDGE('',*,*,#6108,.F.);
#8295=ORIENTED_EDGE('',*,*,#6105,.F.);
#8296=ORIENTED_EDGE('',*,*,#6102,.F.);
#8297=ORIENTED_EDGE('',*,*,#6099,.F.);
#8298=ORIENTED_EDGE('',*,*,#6096,.F.);
#8299=ORIENTED_EDGE('',*,*,#6092,.F.);
#8300=ORIENTED_EDGE('',*,*,#6109,.F.);
#8301=ORIENTED_EDGE('',*,*,#6094,.F.);
#8302=ORIENTED_EDGE('',*,*,#6098,.F.);
#8303=ORIENTED_EDGE('',*,*,#6101,.F.);
#8304=ORIENTED_EDGE('',*,*,#6104,.F.);
#8305=ORIENTED_EDGE('',*,*,#6107,.F.);
#8306=ORIENTED_EDGE('',*,*,#6110,.F.);
#8307=ORIENTED_EDGE('',*,*,#6111,.F.);
#8308=ORIENTED_EDGE('',*,*,#6112,.F.);
#8309=ORIENTED_EDGE('',*,*,#6113,.T.);
#8310=ORIENTED_EDGE('',*,*,#6111,.T.);
#8311=ORIENTED_EDGE('',*,*,#6113,.F.);
#8312=ORIENTED_EDGE('',*,*,#6114,.F.);
#8313=ORIENTED_EDGE('',*,*,#6115,.T.);
#8314=ORIENTED_EDGE('',*,*,#6112,.T.);
#8315=ORIENTED_EDGE('',*,*,#6115,.F.);
#8316=ORIENTED_EDGE('',*,*,#6116,.F.);
#8317=ORIENTED_EDGE('',*,*,#6117,.T.);
#8318=ORIENTED_EDGE('',*,*,#6114,.T.);
#8319=ORIENTED_EDGE('',*,*,#6117,.F.);
#8320=ORIENTED_EDGE('',*,*,#6116,.T.);
#8321=ORIENTED_EDGE('',*,*,#6118,.F.);
#8322=ORIENTED_EDGE('',*,*,#6119,.F.);
#8323=ORIENTED_EDGE('',*,*,#6120,.T.);
#8324=ORIENTED_EDGE('',*,*,#6118,.T.);
#8325=ORIENTED_EDGE('',*,*,#6120,.F.);
#8326=ORIENTED_EDGE('',*,*,#6110,.T.);
#8327=ORIENTED_EDGE('',*,*,#6121,.T.);
#8328=ORIENTED_EDGE('',*,*,#6119,.T.);
#8329=ORIENTED_EDGE('',*,*,#6121,.F.);
#8330=CYLINDRICAL_SURFACE('',#9688,0.164999999999999);
#8331=CYLINDRICAL_SURFACE('',#9691,0.164999999999999);
#8332=CYLINDRICAL_SURFACE('',#9694,0.165);
#8333=CYLINDRICAL_SURFACE('',#9697,0.165);
#8334=CYLINDRICAL_SURFACE('',#9700,0.21);
#8335=CYLINDRICAL_SURFACE('',#9703,0.21);
#8336=CYLINDRICAL_SURFACE('',#9706,0.21);
#8337=CYLINDRICAL_SURFACE('',#9709,0.21);
#8338=CYLINDRICAL_SURFACE('',#9712,0.21);
#8339=CYLINDRICAL_SURFACE('',#9715,0.21);
#8340=CYLINDRICAL_SURFACE('',#9718,0.21);
#8341=CYLINDRICAL_SURFACE('',#9721,0.21);
#8342=CYLINDRICAL_SURFACE('',#9731,0.34);
#8343=CYLINDRICAL_SURFACE('',#9735,0.34);
#8344=CYLINDRICAL_SURFACE('',#9739,0.5);
#8345=CYLINDRICAL_SURFACE('',#9744,0.5);
#8346=CYLINDRICAL_SURFACE('',#9749,0.5);
#8347=CYLINDRICAL_SURFACE('',#9754,0.5);
#8348=CYLINDRICAL_SURFACE('',#9759,0.275);
#8349=CYLINDRICAL_SURFACE('',#9761,0.275);
#8350=CYLINDRICAL_SURFACE('',#9763,0.275);
#8351=CYLINDRICAL_SURFACE('',#9765,0.275);
#8352=CYLINDRICAL_SURFACE('',#9774,0.425);
#8353=CYLINDRICAL_SURFACE('',#9777,0.645);
#8354=CYLINDRICAL_SURFACE('',#9783,0.425);
#8355=CYLINDRICAL_SURFACE('',#9786,0.645);
#8356=CYLINDRICAL_SURFACE('',#9792,0.34);
#8357=CYLINDRICAL_SURFACE('',#9796,0.34);
#8358=CYLINDRICAL_SURFACE('',#9800,0.5);
#8359=CYLINDRICAL_SURFACE('',#9805,0.5);
#8360=CYLINDRICAL_SURFACE('',#9810,0.5);
#8361=CYLINDRICAL_SURFACE('',#9815,0.5);
#8362=CYLINDRICAL_SURFACE('',#9820,0.275);
#8363=CYLINDRICAL_SURFACE('',#9822,0.275);
#8364=CYLINDRICAL_SURFACE('',#9824,0.275);
#8365=CYLINDRICAL_SURFACE('',#9826,0.275);
#8366=CYLINDRICAL_SURFACE('',#9835,0.425);
#8367=CYLINDRICAL_SURFACE('',#9838,0.645);
#8368=CYLINDRICAL_SURFACE('',#9844,0.425);
#8369=CYLINDRICAL_SURFACE('',#9847,0.645);
#8370=CYLINDRICAL_SURFACE('',#9853,0.4);
#8371=CYLINDRICAL_SURFACE('',#9856,0.4);
#8372=CYLINDRICAL_SURFACE('',#9861,0.4);
#8373=CYLINDRICAL_SURFACE('',#9871,0.225);
#8374=CYLINDRICAL_SURFACE('',#9873,0.225);
#8375=CYLINDRICAL_SURFACE('',#9875,0.21);
#8376=CYLINDRICAL_SURFACE('',#9878,0.21);
#8377=CYLINDRICAL_SURFACE('',#9881,0.21);
#8378=CYLINDRICAL_SURFACE('',#9884,0.21);
#8379=CYLINDRICAL_SURFACE('',#9893,0.399999999999999);
#8380=CYLINDRICAL_SURFACE('',#9896,0.399999999999999);
#8381=CYLINDRICAL_SURFACE('',#9901,0.399999999999999);
#8382=CYLINDRICAL_SURFACE('',#9911,0.225000000000001);
#8383=CYLINDRICAL_SURFACE('',#9913,0.225000000000001);
#8384=CYLINDRICAL_SURFACE('',#9915,0.210000000000001);
#8385=CYLINDRICAL_SURFACE('',#9918,0.210000000000001);
#8386=CYLINDRICAL_SURFACE('',#9921,0.210000000000001);
#8387=CYLINDRICAL_SURFACE('',#9924,0.210000000000001);
#8388=CYLINDRICAL_SURFACE('',#9951,0.425);
#8389=CYLINDRICAL_SURFACE('',#9959,0.24505);
#8390=CYLINDRICAL_SURFACE('',#9974,2.05);
#8391=CYLINDRICAL_SURFACE('',#9977,2.05);
#8392=CYLINDRICAL_SURFACE('',#9995,2.8);
#8393=CYLINDRICAL_SURFACE('',#10005,0.65);
#8394=CYLINDRICAL_SURFACE('',#10007,0.65);
#8395=CYLINDRICAL_SURFACE('',#10015,1.8);
#8396=CYLINDRICAL_SURFACE('',#10024,0.25);
#8397=CYLINDRICAL_SURFACE('',#10025,0.25);
#8398=CYLINDRICAL_SURFACE('',#10026,1.65);
#8399=CYLINDRICAL_SURFACE('',#10029,0.25);
#8400=CYLINDRICAL_SURFACE('',#10030,0.25);
#8401=CYLINDRICAL_SURFACE('',#10031,0.25);
#8402=CYLINDRICAL_SURFACE('',#10032,0.25);
#8403=CYLINDRICAL_SURFACE('',#10037,1.75);
#8404=CYLINDRICAL_SURFACE('',#10041,1.);
#8405=CYLINDRICAL_SURFACE('',#10045,0.42);
#8406=CYLINDRICAL_SURFACE('',#10048,0.8);
#8407=CYLINDRICAL_SURFACE('',#10068,0.65);
#8408=CYLINDRICAL_SURFACE('',#10076,0.3933);
#8409=CYLINDRICAL_SURFACE('',#10080,0.525);
#8410=CYLINDRICAL_SURFACE('',#10082,0.525);
#8411=CYLINDRICAL_SURFACE('',#10092,0.225);
#8412=CYLINDRICAL_SURFACE('',#10095,0.165);
#8413=CYLINDRICAL_SURFACE('',#10097,0.275);
#8414=CYLINDRICAL_SURFACE('',#10099,0.275);
#8415=CYLINDRICAL_SURFACE('',#10101,0.6);
#8416=CYLINDRICAL_SURFACE('',#10119,0.265);
#8417=CYLINDRICAL_SURFACE('',#10123,0.5);
#8418=CYLINDRICAL_SURFACE('',#10141,0.425);
#8419=CYLINDRICAL_SURFACE('',#10149,0.24505);
#8420=CYLINDRICAL_SURFACE('',#10155,0.35);
#8421=CYLINDRICAL_SURFACE('',#10163,0.1954);
#8422=CYLINDRICAL_SURFACE('',#10182,0.6);
#8423=CYLINDRICAL_SURFACE('',#10191,1.);
#8424=CYLINDRICAL_SURFACE('',#10200,0.21);
#8425=CYLINDRICAL_SURFACE('',#10204,1.005);
#8426=CYLINDRICAL_SURFACE('',#10207,1.5);
#8427=CYLINDRICAL_SURFACE('',#10215,0.21);
#8428=CYLINDRICAL_SURFACE('',#10219,1.005);
#8429=CYLINDRICAL_SURFACE('',#10222,1.5);
#8430=CYLINDRICAL_SURFACE('',#10228,1.005);
#8431=CYLINDRICAL_SURFACE('',#10231,1.3);
#8432=CYLINDRICAL_SURFACE('',#10237,0.5);
#8433=CYLINDRICAL_SURFACE('',#10243,0.34);
#8434=CYLINDRICAL_SURFACE('',#10249,0.21);
#8435=CYLINDRICAL_SURFACE('',#10252,1.);
#8436=CYLINDRICAL_SURFACE('',#10264,4.);
#8437=CYLINDRICAL_SURFACE('',#10265,1.6);
#8438=CYLINDRICAL_SURFACE('',#10268,1.6);
#8439=CYLINDRICAL_SURFACE('',#10271,0.165);
#8440=CYLINDRICAL_SURFACE('',#10278,0.5);
#8441=CYLINDRICAL_SURFACE('',#10281,0.4);
#8442=CYLINDRICAL_SURFACE('',#10285,0.505);
#8443=CYLINDRICAL_SURFACE('',#10288,0.7);
#8444=CYLINDRICAL_SURFACE('',#10294,0.505);
#8445=CYLINDRICAL_SURFACE('',#10297,0.7);
#8446=CYLINDRICAL_SURFACE('',#10303,0.225);
#8447=CYLINDRICAL_SURFACE('',#10306,0.8);
#8448=CYLINDRICAL_SURFACE('',#10334,0.24505);
#8449=CYLINDRICAL_SURFACE('',#10341,1.5);
#8450=CYLINDRICAL_SURFACE('',#10344,1.5);
#8451=CYLINDRICAL_SURFACE('',#10347,2.);
#8452=CYLINDRICAL_SURFACE('',#10353,2.);
#8453=CYLINDRICAL_SURFACE('',#10358,1.1);
#8454=CYLINDRICAL_SURFACE('',#10361,2.);
#8455=CYLINDRICAL_SURFACE('',#10367,1.1);
#8456=CYLINDRICAL_SURFACE('',#10370,2.);
#8457=CYLINDRICAL_SURFACE('',#10376,1.1);
#8458=CYLINDRICAL_SURFACE('',#10379,2.);
#8459=CYLINDRICAL_SURFACE('',#10385,1.1);
#8460=CYLINDRICAL_SURFACE('',#10388,2.);
#8461=CYLINDRICAL_SURFACE('',#10401,0.976185);
#8462=CYLINDRICAL_SURFACE('',#10403,0.5);
#8463=CYLINDRICAL_SURFACE('',#10409,0.976185);
#8464=CYLINDRICAL_SURFACE('',#10421,1.023815);
#8465=CYLINDRICAL_SURFACE('',#10428,1.5);
#8466=CYLINDRICAL_SURFACE('',#10433,1.023815);
#8467=CYLINDRICAL_SURFACE('',#10455,1.019052);
#8468=CYLINDRICAL_SURFACE('',#10495,0.980948);
#8469=CYLINDRICAL_SURFACE('',#10509,1.013815);
#8470=CYLINDRICAL_SURFACE('',#10513,0.991185);
#8471=CYLINDRICAL_SURFACE('',#10517,1.013815);
#8472=CYLINDRICAL_SURFACE('',#10521,0.991185);
#8473=CYLINDRICAL_SURFACE('',#10536,0.5);
#8474=CYLINDRICAL_SURFACE('',#10544,0.165);
#8475=CYLINDRICAL_SURFACE('',#10547,0.165);
#8476=CYLINDRICAL_SURFACE('',#10550,0.165);
#8477=CYLINDRICAL_SURFACE('',#10553,0.165);
#8478=CYLINDRICAL_SURFACE('',#10556,1.05);
#8479=CYLINDRICAL_SURFACE('',#10559,1.05);
#8480=CYLINDRICAL_SURFACE('',#10569,0.225);
#8481=CYLINDRICAL_SURFACE('',#10572,0.225);
#8482=CYLINDRICAL_SURFACE('',#10575,0.225);
#8483=CYLINDRICAL_SURFACE('',#10578,0.225);
#8484=CYLINDRICAL_SURFACE('',#10581,0.7);
#8485=CYLINDRICAL_SURFACE('',#10584,0.7);
#8486=CYLINDRICAL_SURFACE('',#10594,0.225);
#8487=CYLINDRICAL_SURFACE('',#10597,0.225);
#8488=CYLINDRICAL_SURFACE('',#10600,0.225);
#8489=CYLINDRICAL_SURFACE('',#10603,0.225);
#8490=CYLINDRICAL_SURFACE('',#10606,0.7);
#8491=CYLINDRICAL_SURFACE('',#10609,0.7);
#8492=CYLINDRICAL_SURFACE('',#10619,0.164999999999999);
#8493=CYLINDRICAL_SURFACE('',#10626,0.800000000000001);
#8494=CYLINDRICAL_SURFACE('',#10629,0.5);
#8495=CYLINDRICAL_SURFACE('',#10633,0.505000000000001);
#8496=CYLINDRICAL_SURFACE('',#10636,0.699999999999999);
#8497=CYLINDRICAL_SURFACE('',#10642,0.505000000000001);
#8498=CYLINDRICAL_SURFACE('',#10645,0.699999999999999);
#8499=CYLINDRICAL_SURFACE('',#10651,0.225);
#8500=CYLINDRICAL_SURFACE('',#10654,0.800000000000001);
#8501=CYLINDRICAL_SURFACE('',#10671,1.05);
#8502=CYLINDRICAL_SURFACE('',#10675,1.);
#8503=CYLINDRICAL_SURFACE('',#10679,1.05);
#8504=CYLINDRICAL_SURFACE('',#10683,1.);
#8505=CYLINDRICAL_SURFACE('',#10687,1.05);
#8506=CYLINDRICAL_SURFACE('',#10691,0.9);
#8507=CYLINDRICAL_SURFACE('',#10704,0.895);
#8508=CYLINDRICAL_SURFACE('',#10708,0.605);
#8509=CYLINDRICAL_SURFACE('',#10726,0.35);
#8510=CYLINDRICAL_SURFACE('',#10734,0.1954);
#8511=ADVANCED_FACE('',(#1320),#8330,.F.);
#8512=ADVANCED_FACE('',(#1321),#8331,.F.);
#8513=ADVANCED_FACE('',(#1322),#8332,.F.);
#8514=ADVANCED_FACE('',(#1323),#8333,.F.);
#8515=ADVANCED_FACE('',(#1324),#8334,.F.);
#8516=ADVANCED_FACE('',(#1325),#8335,.F.);
#8517=ADVANCED_FACE('',(#1326),#8336,.F.);
#8518=ADVANCED_FACE('',(#1327),#8337,.F.);
#8519=ADVANCED_FACE('',(#1328),#8338,.F.);
#8520=ADVANCED_FACE('',(#1329),#8339,.F.);
#8521=ADVANCED_FACE('',(#1330),#8340,.F.);
#8522=ADVANCED_FACE('',(#1331),#8341,.F.);
#8523=ADVANCED_FACE('',(#1332),#1011,.T.);
#8524=ADVANCED_FACE('',(#1333),#1012,.T.);
#8525=ADVANCED_FACE('',(#1334),#1013,.T.);
#8526=ADVANCED_FACE('',(#1335),#1014,.T.);
#8527=ADVANCED_FACE('',(#1336,#785,#786,#787,#788,#789,#790,#791,#792,#793,
#794,#795,#796),#1015,.T.);
#8528=ADVANCED_FACE('',(#1337,#797,#798,#799,#800,#801,#802,#803,#804,#805,
#806,#807,#808),#1016,.F.);
#8529=ADVANCED_FACE('',(#1338),#8342,.F.);
#8530=ADVANCED_FACE('',(#1339),#1017,.T.);
#8531=ADVANCED_FACE('',(#1340),#8343,.F.);
#8532=ADVANCED_FACE('',(#1341),#1018,.T.);
#8533=ADVANCED_FACE('',(#1342),#8344,.F.);
#8534=ADVANCED_FACE('',(#1343,#809),#1019,.T.);
#8535=ADVANCED_FACE('',(#1344),#8345,.F.);
#8536=ADVANCED_FACE('',(#1345,#810),#1020,.T.);
#8537=ADVANCED_FACE('',(#1346),#8346,.F.);
#8538=ADVANCED_FACE('',(#1347,#811),#1021,.T.);
#8539=ADVANCED_FACE('',(#1348),#8347,.F.);
#8540=ADVANCED_FACE('',(#1349,#812),#1022,.T.);
#8541=ADVANCED_FACE('',(#1350),#8348,.F.);
#8542=ADVANCED_FACE('',(#1351),#8349,.F.);
#8543=ADVANCED_FACE('',(#1352),#8350,.F.);
#8544=ADVANCED_FACE('',(#1353),#8351,.F.);
#8545=ADVANCED_FACE('',(#1354),#1023,.T.);
#8546=ADVANCED_FACE('',(#1355),#1024,.T.);
#8547=ADVANCED_FACE('',(#1356),#1025,.T.);
#8548=ADVANCED_FACE('',(#1357),#1026,.T.);
#8549=ADVANCED_FACE('',(#1358,#813,#814,#815,#816,#817,#818),#1027,.T.);
#8550=ADVANCED_FACE('',(#1359,#819,#820,#821,#822),#1028,.F.);
#8551=ADVANCED_FACE('',(#1360),#8352,.F.);
#8552=ADVANCED_FACE('',(#1361),#8353,.T.);
#8553=ADVANCED_FACE('',(#1362,#823),#1029,.T.);
#8554=ADVANCED_FACE('',(#1363,#824),#1030,.F.);
#8555=ADVANCED_FACE('',(#1364),#8354,.F.);
#8556=ADVANCED_FACE('',(#1365),#8355,.T.);
#8557=ADVANCED_FACE('',(#1366,#825),#1031,.T.);
#8558=ADVANCED_FACE('',(#1367,#826),#1032,.F.);
#8559=ADVANCED_FACE('',(#1368),#8356,.F.);
#8560=ADVANCED_FACE('',(#1369),#1033,.T.);
#8561=ADVANCED_FACE('',(#1370),#8357,.F.);
#8562=ADVANCED_FACE('',(#1371),#1034,.T.);
#8563=ADVANCED_FACE('',(#1372),#8358,.F.);
#8564=ADVANCED_FACE('',(#1373,#827),#1035,.T.);
#8565=ADVANCED_FACE('',(#1374),#8359,.F.);
#8566=ADVANCED_FACE('',(#1375,#828),#1036,.T.);
#8567=ADVANCED_FACE('',(#1376),#8360,.F.);
#8568=ADVANCED_FACE('',(#1377,#829),#1037,.T.);
#8569=ADVANCED_FACE('',(#1378),#8361,.F.);
#8570=ADVANCED_FACE('',(#1379,#830),#1038,.T.);
#8571=ADVANCED_FACE('',(#1380),#8362,.F.);
#8572=ADVANCED_FACE('',(#1381),#8363,.F.);
#8573=ADVANCED_FACE('',(#1382),#8364,.F.);
#8574=ADVANCED_FACE('',(#1383),#8365,.F.);
#8575=ADVANCED_FACE('',(#1384),#1039,.T.);
#8576=ADVANCED_FACE('',(#1385),#1040,.T.);
#8577=ADVANCED_FACE('',(#1386),#1041,.T.);
#8578=ADVANCED_FACE('',(#1387),#1042,.T.);
#8579=ADVANCED_FACE('',(#1388,#831,#832,#833,#834,#835,#836),#1043,.T.);
#8580=ADVANCED_FACE('',(#1389,#837,#838,#839,#840),#1044,.F.);
#8581=ADVANCED_FACE('',(#1390),#8366,.F.);
#8582=ADVANCED_FACE('',(#1391),#8367,.T.);
#8583=ADVANCED_FACE('',(#1392,#841),#1045,.T.);
#8584=ADVANCED_FACE('',(#1393,#842),#1046,.F.);
#8585=ADVANCED_FACE('',(#1394),#8368,.F.);
#8586=ADVANCED_FACE('',(#1395),#8369,.T.);
#8587=ADVANCED_FACE('',(#1396,#843),#1047,.T.);
#8588=ADVANCED_FACE('',(#1397,#844),#1048,.F.);
#8589=ADVANCED_FACE('',(#1398),#8370,.F.);
#8590=ADVANCED_FACE('',(#1399),#8371,.F.);
#8591=ADVANCED_FACE('',(#1400,#845),#1049,.T.);
#8592=ADVANCED_FACE('',(#1401),#8372,.F.);
#8593=ADVANCED_FACE('',(#1402,#846),#1050,.T.);
#8594=ADVANCED_FACE('',(#1403,#847,#848,#849,#850),#1051,.T.);
#8595=ADVANCED_FACE('',(#1404),#8373,.F.);
#8596=ADVANCED_FACE('',(#1405),#8374,.F.);
#8597=ADVANCED_FACE('',(#1406),#8375,.F.);
#8598=ADVANCED_FACE('',(#1407),#1052,.T.);
#8599=ADVANCED_FACE('',(#1408),#8376,.F.);
#8600=ADVANCED_FACE('',(#1409),#1053,.T.);
#8601=ADVANCED_FACE('',(#1410),#8377,.F.);
#8602=ADVANCED_FACE('',(#1411),#1054,.T.);
#8603=ADVANCED_FACE('',(#1412),#8378,.F.);
#8604=ADVANCED_FACE('',(#1413),#1055,.T.);
#8605=ADVANCED_FACE('',(#1414),#1056,.T.);
#8606=ADVANCED_FACE('',(#1415),#1057,.T.);
#8607=ADVANCED_FACE('',(#1416),#1058,.T.);
#8608=ADVANCED_FACE('',(#1417),#1059,.T.);
#8609=ADVANCED_FACE('',(#1418,#851,#852),#1060,.F.);
#8610=ADVANCED_FACE('',(#1419),#8379,.F.);
#8611=ADVANCED_FACE('',(#1420),#8380,.F.);
#8612=ADVANCED_FACE('',(#1421,#853),#1061,.T.);
#8613=ADVANCED_FACE('',(#1422),#8381,.F.);
#8614=ADVANCED_FACE('',(#1423,#854),#1062,.T.);
#8615=ADVANCED_FACE('',(#1424,#855,#856,#857,#858),#1063,.T.);
#8616=ADVANCED_FACE('',(#1425),#8382,.F.);
#8617=ADVANCED_FACE('',(#1426),#8383,.F.);
#8618=ADVANCED_FACE('',(#1427),#8384,.F.);
#8619=ADVANCED_FACE('',(#1428),#1064,.T.);
#8620=ADVANCED_FACE('',(#1429),#8385,.F.);
#8621=ADVANCED_FACE('',(#1430),#1065,.T.);
#8622=ADVANCED_FACE('',(#1431),#8386,.F.);
#8623=ADVANCED_FACE('',(#1432),#1066,.T.);
#8624=ADVANCED_FACE('',(#1433),#8387,.F.);
#8625=ADVANCED_FACE('',(#1434),#1067,.T.);
#8626=ADVANCED_FACE('',(#1435),#1068,.T.);
#8627=ADVANCED_FACE('',(#1436),#1069,.T.);
#8628=ADVANCED_FACE('',(#1437),#1070,.T.);
#8629=ADVANCED_FACE('',(#1438),#1071,.T.);
#8630=ADVANCED_FACE('',(#1439,#859,#860),#1072,.F.);
#8631=ADVANCED_FACE('',(#1440),#1073,.T.);
#8632=ADVANCED_FACE('',(#1441),#1074,.T.);
#8633=ADVANCED_FACE('',(#1442),#1075,.T.);
#8634=ADVANCED_FACE('',(#1443),#1076,.T.);
#8635=ADVANCED_FACE('',(#1444),#1077,.T.);
#8636=ADVANCED_FACE('',(#1445),#1078,.F.);
#8637=ADVANCED_FACE('',(#1446),#1079,.T.);
#8638=ADVANCED_FACE('',(#1447),#1080,.T.);
#8639=ADVANCED_FACE('',(#1448),#1081,.T.);
#8640=ADVANCED_FACE('',(#1449),#1082,.T.);
#8641=ADVANCED_FACE('',(#1450),#1083,.T.);
#8642=ADVANCED_FACE('',(#1451),#1084,.F.);
#8643=ADVANCED_FACE('',(#1452),#1085,.T.);
#8644=ADVANCED_FACE('',(#1453),#534,.T.);
#8645=ADVANCED_FACE('',(#1454),#8388,.T.);
#8646=ADVANCED_FACE('',(#1455),#535,.T.);
#8647=ADVANCED_FACE('',(#1456,#861),#1086,.T.);
#8648=ADVANCED_FACE('',(#1457),#536,.T.);
#8649=ADVANCED_FACE('',(#1458),#8389,.T.);
#8650=ADVANCED_FACE('',(#1459),#537,.T.);
#8651=ADVANCED_FACE('',(#1460),#1087,.T.);
#8652=ADVANCED_FACE('',(#1461),#1088,.F.);
#8653=ADVANCED_FACE('',(#1462),#1089,.F.);
#8654=ADVANCED_FACE('',(#1463),#1090,.F.);
#8655=ADVANCED_FACE('',(#1464),#1091,.F.);
#8656=ADVANCED_FACE('',(#1465),#1092,.F.);
#8657=ADVANCED_FACE('',(#1466),#1093,.F.);
#8658=ADVANCED_FACE('',(#1467),#1094,.F.);
#8659=ADVANCED_FACE('',(#1468),#1095,.F.);
#8660=ADVANCED_FACE('',(#1469),#8390,.F.);
#8661=ADVANCED_FACE('',(#1470),#8391,.F.);
#8662=ADVANCED_FACE('',(#1471,#862,#863),#511,.F.);
#8663=ADVANCED_FACE('',(#1472),#1096,.T.);
#8664=ADVANCED_FACE('',(#1473),#1097,.T.);
#8665=ADVANCED_FACE('',(#1474),#1098,.T.);
#8666=ADVANCED_FACE('',(#1475),#1099,.T.);
#8667=ADVANCED_FACE('',(#1476),#1100,.T.);
#8668=ADVANCED_FACE('',(#1477),#1101,.T.);
#8669=ADVANCED_FACE('',(#1478,#864,#865,#866),#1102,.T.);
#8670=ADVANCED_FACE('',(#1479),#8392,.T.);
#8671=ADVANCED_FACE('',(#1480,#867),#1103,.F.);
#8672=ADVANCED_FACE('',(#1481,#868),#1104,.T.);
#8673=ADVANCED_FACE('',(#1482),#1105,.F.);
#8674=ADVANCED_FACE('',(#1483),#1106,.F.);
#8675=ADVANCED_FACE('',(#1484),#1107,.F.);
#8676=ADVANCED_FACE('',(#1485),#1108,.F.);
#8677=ADVANCED_FACE('',(#1486),#1109,.F.);
#8678=ADVANCED_FACE('',(#1487),#8393,.F.);
#8679=ADVANCED_FACE('',(#1488),#8394,.F.);
#8680=ADVANCED_FACE('',(#1489),#1110,.T.);
#8681=ADVANCED_FACE('',(#1490),#1111,.T.);
#8682=ADVANCED_FACE('',(#1491),#1112,.T.);
#8683=ADVANCED_FACE('',(#1492),#1113,.T.);
#8684=ADVANCED_FACE('',(#1493,#869,#870,#871),#1114,.F.);
#8685=ADVANCED_FACE('',(#1494),#8395,.F.);
#8686=ADVANCED_FACE('',(#1495,#872),#1115,.T.);
#8687=ADVANCED_FACE('',(#1496,#873,#874),#512,.T.);
#8688=ADVANCED_FACE('',(#1497,#875),#1116,.T.);
#8689=ADVANCED_FACE('',(#1498),#8396,.F.);
#8690=ADVANCED_FACE('',(#1499),#8397,.F.);
#8691=ADVANCED_FACE('',(#1500,#876,#877,#878,#879,#880,#881),#8398,.T.);
#8692=ADVANCED_FACE('',(#1501),#8399,.F.);
#8693=ADVANCED_FACE('',(#1502),#8400,.F.);
#8694=ADVANCED_FACE('',(#1503),#8401,.F.);
#8695=ADVANCED_FACE('',(#1504),#8402,.F.);
#8696=ADVANCED_FACE('',(#1505,#882),#1117,.T.);
#8697=ADVANCED_FACE('',(#1506,#883),#1118,.T.);
#8698=ADVANCED_FACE('',(#1507),#8403,.T.);
#8699=ADVANCED_FACE('',(#1508,#884),#1119,.T.);
#8700=ADVANCED_FACE('',(#1509,#885,#886,#887,#888,#889,#890),#8404,.F.);
#8701=ADVANCED_FACE('',(#1510),#8405,.F.);
#8702=ADVANCED_FACE('',(#1511),#8406,.T.);
#8703=ADVANCED_FACE('',(#1512,#891),#1120,.T.);
#8704=ADVANCED_FACE('',(#1513,#892),#1121,.F.);
#8705=ADVANCED_FACE('',(#1514),#1122,.F.);
#8706=ADVANCED_FACE('',(#1515),#1123,.F.);
#8707=ADVANCED_FACE('',(#1516),#1124,.F.);
#8708=ADVANCED_FACE('',(#1517),#1125,.F.);
#8709=ADVANCED_FACE('',(#1518),#1126,.F.);
#8710=ADVANCED_FACE('',(#1519),#1127,.F.);
#8711=ADVANCED_FACE('',(#1520),#1128,.F.);
#8712=ADVANCED_FACE('',(#1521),#1129,.F.);
#8713=ADVANCED_FACE('',(#1522),#1130,.F.);
#8714=ADVANCED_FACE('',(#1523),#1131,.T.);
#8715=ADVANCED_FACE('',(#1524),#538,.T.);
#8716=ADVANCED_FACE('',(#1525),#8407,.T.);
#8717=ADVANCED_FACE('',(#1526),#539,.T.);
#8718=ADVANCED_FACE('',(#1527,#893),#1132,.T.);
#8719=ADVANCED_FACE('',(#1528),#540,.T.);
#8720=ADVANCED_FACE('',(#1529),#8408,.T.);
#8721=ADVANCED_FACE('',(#1530),#1133,.F.);
#8722=ADVANCED_FACE('',(#1531),#8409,.F.);
#8723=ADVANCED_FACE('',(#1532),#8410,.F.);
#8724=ADVANCED_FACE('',(#1533),#1134,.F.);
#8725=ADVANCED_FACE('',(#1534,#894),#1135,.T.);
#8726=ADVANCED_FACE('',(#1535,#895),#1136,.T.);
#8727=ADVANCED_FACE('',(#1536,#896),#1137,.T.);
#8728=ADVANCED_FACE('',(#1537),#8411,.F.);
#8729=ADVANCED_FACE('',(#1538),#8412,.F.);
#8730=ADVANCED_FACE('',(#1539),#8413,.F.);
#8731=ADVANCED_FACE('',(#1540),#8414,.F.);
#8732=ADVANCED_FACE('',(#1541),#8415,.F.);
#8733=ADVANCED_FACE('',(#1542,#897),#1138,.T.);
#8734=ADVANCED_FACE('',(#1543),#1139,.T.);
#8735=ADVANCED_FACE('',(#1544,#898,#899),#1140,.T.);
#8736=ADVANCED_FACE('',(#1545),#1141,.T.);
#8737=ADVANCED_FACE('',(#1546,#900),#1142,.T.);
#8738=ADVANCED_FACE('',(#1547),#1143,.T.);
#8739=ADVANCED_FACE('',(#1548,#901),#1144,.T.);
#8740=ADVANCED_FACE('',(#1549),#1145,.T.);
#8741=ADVANCED_FACE('',(#1550,#902),#1146,.T.);
#8742=ADVANCED_FACE('',(#1551),#1147,.T.);
#8743=ADVANCED_FACE('',(#1552,#903),#1148,.T.);
#8744=ADVANCED_FACE('',(#1553),#541,.F.);
#8745=ADVANCED_FACE('',(#1554),#8416,.F.);
#8746=ADVANCED_FACE('',(#1555,#904),#1149,.T.);
#8747=ADVANCED_FACE('',(#1556),#8417,.T.);
#8748=ADVANCED_FACE('',(#1557,#905),#1150,.F.);
#8749=ADVANCED_FACE('',(#1558),#1151,.F.);
#8750=ADVANCED_FACE('',(#1559),#1152,.F.);
#8751=ADVANCED_FACE('',(#1560),#1153,.F.);
#8752=ADVANCED_FACE('',(#1561),#1154,.F.);
#8753=ADVANCED_FACE('',(#1562),#1155,.F.);
#8754=ADVANCED_FACE('',(#1563),#1156,.F.);
#8755=ADVANCED_FACE('',(#1564),#1157,.F.);
#8756=ADVANCED_FACE('',(#1565),#1158,.F.);
#8757=ADVANCED_FACE('',(#1566),#1159,.F.);
#8758=ADVANCED_FACE('',(#1567),#1160,.T.);
#8759=ADVANCED_FACE('',(#1568),#542,.T.);
#8760=ADVANCED_FACE('',(#1569),#8418,.T.);
#8761=ADVANCED_FACE('',(#1570),#543,.T.);
#8762=ADVANCED_FACE('',(#1571,#906),#1161,.T.);
#8763=ADVANCED_FACE('',(#1572),#544,.T.);
#8764=ADVANCED_FACE('',(#1573),#8419,.T.);
#8765=ADVANCED_FACE('',(#1574),#1162,.T.);
#8766=ADVANCED_FACE('',(#1575),#545,.T.);
#8767=ADVANCED_FACE('',(#1576),#8420,.T.);
#8768=ADVANCED_FACE('',(#1577),#546,.T.);
#8769=ADVANCED_FACE('',(#1578,#907),#1163,.T.);
#8770=ADVANCED_FACE('',(#1579),#547,.T.);
#8771=ADVANCED_FACE('',(#1580),#8421,.T.);
#8772=ADVANCED_FACE('',(#1581),#548,.T.);
#8773=ADVANCED_FACE('',(#1582),#1164,.T.);
#8774=ADVANCED_FACE('',(#1583),#1165,.F.);
#8775=ADVANCED_FACE('',(#1584),#1166,.F.);
#8776=ADVANCED_FACE('',(#1585),#1167,.F.);
#8777=ADVANCED_FACE('',(#1586),#1168,.F.);
#8778=ADVANCED_FACE('',(#1587),#1169,.F.);
#8779=ADVANCED_FACE('',(#1588),#1170,.F.);
#8780=ADVANCED_FACE('',(#1589),#1171,.F.);
#8781=ADVANCED_FACE('',(#1590),#1172,.F.);
#8782=ADVANCED_FACE('',(#1591),#1173,.T.);
#8783=ADVANCED_FACE('',(#1592),#549,.T.);
#8784=ADVANCED_FACE('',(#1593),#8422,.T.);
#8785=ADVANCED_FACE('',(#1594),#1174,.F.);
#8786=ADVANCED_FACE('',(#1595),#1175,.F.);
#8787=ADVANCED_FACE('',(#1596),#1176,.T.);
#8788=ADVANCED_FACE('',(#1597),#1177,.F.);
#8789=ADVANCED_FACE('',(#1598),#1178,.F.);
#8790=ADVANCED_FACE('',(#1599),#8423,.T.);
#8791=ADVANCED_FACE('',(#1600),#1179,.T.);
#8792=ADVANCED_FACE('',(#1601),#1180,.F.);
#8793=ADVANCED_FACE('',(#1602),#1181,.T.);
#8794=ADVANCED_FACE('',(#1603),#8424,.F.);
#8795=ADVANCED_FACE('',(#1604),#1182,.T.);
#8796=ADVANCED_FACE('',(#1605,#908),#8425,.F.);
#8797=ADVANCED_FACE('',(#1606,#909),#8426,.T.);
#8798=ADVANCED_FACE('',(#1607,#910),#1183,.T.);
#8799=ADVANCED_FACE('',(#1608,#911),#1184,.F.);
#8800=ADVANCED_FACE('',(#1609),#1185,.T.);
#8801=ADVANCED_FACE('',(#1610),#8427,.F.);
#8802=ADVANCED_FACE('',(#1611),#1186,.T.);
#8803=ADVANCED_FACE('',(#1612,#912),#8428,.F.);
#8804=ADVANCED_FACE('',(#1613,#913),#8429,.T.);
#8805=ADVANCED_FACE('',(#1614,#914),#1187,.T.);
#8806=ADVANCED_FACE('',(#1615,#915),#1188,.F.);
#8807=ADVANCED_FACE('',(#1616),#8430,.F.);
#8808=ADVANCED_FACE('',(#1617),#8431,.T.);
#8809=ADVANCED_FACE('',(#1618,#916),#1189,.T.);
#8810=ADVANCED_FACE('',(#1619,#917),#1190,.F.);
#8811=ADVANCED_FACE('',(#1620),#8432,.F.);
#8812=ADVANCED_FACE('',(#1621,#918),#1191,.T.);
#8813=ADVANCED_FACE('',(#1622),#8433,.F.);
#8814=ADVANCED_FACE('',(#1623),#1192,.T.);
#8815=ADVANCED_FACE('',(#1624),#1193,.T.);
#8816=ADVANCED_FACE('',(#1625),#8434,.F.);
#8817=ADVANCED_FACE('',(#1626),#1194,.T.);
#8818=ADVANCED_FACE('',(#1627),#8435,.F.);
#8819=ADVANCED_FACE('',(#1628),#1195,.F.);
#8820=ADVANCED_FACE('',(#1629),#1196,.F.);
#8821=ADVANCED_FACE('',(#1630),#1197,.F.);
#8822=ADVANCED_FACE('',(#1631,#919,#920),#1198,.T.);
#8823=ADVANCED_FACE('',(#1632,#921),#1199,.F.);
#8824=ADVANCED_FACE('',(#1633),#8436,.T.);
#8825=ADVANCED_FACE('',(#1634),#8437,.T.);
#8826=ADVANCED_FACE('',(#1635),#8438,.T.);
#8827=ADVANCED_FACE('',(#1636),#1200,.F.);
#8828=ADVANCED_FACE('',(#1637),#8439,.F.);
#8829=ADVANCED_FACE('',(#1638),#1201,.T.);
#8830=ADVANCED_FACE('',(#1639,#922),#1202,.F.);
#8831=ADVANCED_FACE('',(#1640),#8440,.T.);
#8832=ADVANCED_FACE('',(#1641,#923),#1203,.T.);
#8833=ADVANCED_FACE('',(#1642),#8441,.T.);
#8834=ADVANCED_FACE('',(#1643),#1204,.F.);
#8835=ADVANCED_FACE('',(#1644),#8442,.F.);
#8836=ADVANCED_FACE('',(#1645),#8443,.T.);
#8837=ADVANCED_FACE('',(#1646,#924),#1205,.T.);
#8838=ADVANCED_FACE('',(#1647,#925),#1206,.F.);
#8839=ADVANCED_FACE('',(#1648),#8444,.F.);
#8840=ADVANCED_FACE('',(#1649),#8445,.T.);
#8841=ADVANCED_FACE('',(#1650,#926),#1207,.T.);
#8842=ADVANCED_FACE('',(#1651,#927),#1208,.F.);
#8843=ADVANCED_FACE('',(#1652),#8446,.F.);
#8844=ADVANCED_FACE('',(#1653),#8447,.T.);
#8845=ADVANCED_FACE('',(#1654,#928),#1209,.T.);
#8846=ADVANCED_FACE('',(#1655,#929),#1210,.F.);
#8847=ADVANCED_FACE('',(#1656),#1211,.F.);
#8848=ADVANCED_FACE('',(#1657),#1212,.T.);
#8849=ADVANCED_FACE('',(#1658),#1213,.T.);
#8850=ADVANCED_FACE('',(#1659),#1214,.T.);
#8851=ADVANCED_FACE('',(#1660),#1215,.T.);
#8852=ADVANCED_FACE('',(#1661),#1216,.T.);
#8853=ADVANCED_FACE('',(#1662),#1217,.F.);
#8854=ADVANCED_FACE('',(#1663),#1218,.T.);
#8855=ADVANCED_FACE('',(#1664),#1219,.T.);
#8856=ADVANCED_FACE('',(#1665),#1220,.T.);
#8857=ADVANCED_FACE('',(#1666),#1221,.F.);
#8858=ADVANCED_FACE('',(#1667),#1222,.F.);
#8859=ADVANCED_FACE('',(#1668),#1223,.F.);
#8860=ADVANCED_FACE('',(#1669),#1224,.F.);
#8861=ADVANCED_FACE('',(#1670),#1225,.F.);
#8862=ADVANCED_FACE('',(#1671),#1226,.F.);
#8863=ADVANCED_FACE('',(#1672),#1227,.F.);
#8864=ADVANCED_FACE('',(#1673,#930),#1228,.T.);
#8865=ADVANCED_FACE('',(#1674),#550,.T.);
#8866=ADVANCED_FACE('',(#1675),#8448,.T.);
#8867=ADVANCED_FACE('',(#1676),#551,.T.);
#8868=ADVANCED_FACE('',(#1677),#1229,.T.);
#8869=ADVANCED_FACE('',(#1678),#8449,.F.);
#8870=ADVANCED_FACE('',(#1679),#8450,.F.);
#8871=ADVANCED_FACE('',(#1680),#8451,.T.);
#8872=ADVANCED_FACE('',(#1681,#931,#932),#1230,.T.);
#8873=ADVANCED_FACE('',(#1682),#1231,.T.);
#8874=ADVANCED_FACE('',(#1683),#8452,.T.);
#8875=ADVANCED_FACE('',(#1684),#1232,.T.);
#8876=ADVANCED_FACE('',(#1685,#933,#934),#1233,.F.);
#8877=ADVANCED_FACE('',(#1686),#8453,.F.);
#8878=ADVANCED_FACE('',(#1687),#8454,.T.);
#8879=ADVANCED_FACE('',(#1688,#935),#1234,.T.);
#8880=ADVANCED_FACE('',(#1689,#936),#1235,.F.);
#8881=ADVANCED_FACE('',(#1690),#8455,.F.);
#8882=ADVANCED_FACE('',(#1691),#8456,.T.);
#8883=ADVANCED_FACE('',(#1692,#937),#1236,.T.);
#8884=ADVANCED_FACE('',(#1693,#938),#1237,.F.);
#8885=ADVANCED_FACE('',(#1694),#8457,.F.);
#8886=ADVANCED_FACE('',(#1695),#8458,.T.);
#8887=ADVANCED_FACE('',(#1696,#939),#1238,.T.);
#8888=ADVANCED_FACE('',(#1697,#940),#1239,.F.);
#8889=ADVANCED_FACE('',(#1698),#8459,.F.);
#8890=ADVANCED_FACE('',(#1699),#8460,.T.);
#8891=ADVANCED_FACE('',(#1700,#941),#1240,.T.);
#8892=ADVANCED_FACE('',(#1701,#942),#1241,.F.);
#8893=ADVANCED_FACE('',(#1702),#11,.F.);
#8894=ADVANCED_FACE('',(#1703),#8461,.T.);
#8895=ADVANCED_FACE('',(#1704),#8462,.F.);
#8896=ADVANCED_FACE('',(#1705),#552,.F.);
#8897=ADVANCED_FACE('',(#1706,#943),#1242,.T.);
#8898=ADVANCED_FACE('',(#1707),#8463,.T.);
#8899=ADVANCED_FACE('',(#1708,#944),#1243,.T.);
#8900=ADVANCED_FACE('',(#1709),#553,.F.);
#8901=ADVANCED_FACE('',(#1710),#12,.F.);
#8902=ADVANCED_FACE('',(#1711),#8464,.F.);
#8903=ADVANCED_FACE('',(#1712,#945),#1244,.T.);
#8904=ADVANCED_FACE('',(#1713),#554,.T.);
#8905=ADVANCED_FACE('',(#1714),#8465,.T.);
#8906=ADVANCED_FACE('',(#1715),#555,.T.);
#8907=ADVANCED_FACE('',(#1716,#946),#1245,.T.);
#8908=ADVANCED_FACE('',(#1717),#8466,.F.);
#8909=ADVANCED_FACE('',(#1718),#513,.T.);
#8910=ADVANCED_FACE('',(#1719),#514,.T.);
#8911=ADVANCED_FACE('',(#1720),#515,.T.);
#8912=ADVANCED_FACE('',(#1721),#516,.T.);
#8913=ADVANCED_FACE('',(#1722),#517,.T.);
#8914=ADVANCED_FACE('',(#1723),#518,.T.);
#8915=ADVANCED_FACE('',(#1724),#519,.T.);
#8916=ADVANCED_FACE('',(#1725),#520,.T.);
#8917=ADVANCED_FACE('',(#1726),#521,.F.);
#8918=ADVANCED_FACE('',(#1727),#8467,.T.);
#8919=ADVANCED_FACE('',(#1728),#1246,.T.);
#8920=ADVANCED_FACE('',(#1729),#522,.F.);
#8921=ADVANCED_FACE('',(#1730),#1247,.T.);
#8922=ADVANCED_FACE('',(#1731),#523,.F.);
#8923=ADVANCED_FACE('',(#1732),#1248,.T.);
#8924=ADVANCED_FACE('',(#1733),#524,.F.);
#8925=ADVANCED_FACE('',(#1734),#1249,.T.);
#8926=ADVANCED_FACE('',(#1735),#525,.F.);
#8927=ADVANCED_FACE('',(#1736),#1250,.T.);
#8928=ADVANCED_FACE('',(#1737),#526,.F.);
#8929=ADVANCED_FACE('',(#1738),#1251,.T.);
#8930=ADVANCED_FACE('',(#1739),#527,.F.);
#8931=ADVANCED_FACE('',(#1740),#8468,.F.);
#8932=ADVANCED_FACE('',(#1741),#1252,.T.);
#8933=ADVANCED_FACE('',(#1742),#528,.F.);
#8934=ADVANCED_FACE('',(#1743,#947),#1253,.T.);
#8935=ADVANCED_FACE('',(#1744),#1254,.T.);
#8936=ADVANCED_FACE('',(#1745,#948),#1255,.T.);
#8937=ADVANCED_FACE('',(#1746),#8469,.T.);
#8938=ADVANCED_FACE('',(#1747,#949),#1256,.T.);
#8939=ADVANCED_FACE('',(#1748),#8470,.F.);
#8940=ADVANCED_FACE('',(#1749,#950),#1257,.T.);
#8941=ADVANCED_FACE('',(#1750),#8471,.T.);
#8942=ADVANCED_FACE('',(#1751,#951),#1258,.T.);
#8943=ADVANCED_FACE('',(#1752),#8472,.F.);
#8944=ADVANCED_FACE('',(#1753),#8473,.F.);
#8945=ADVANCED_FACE('',(#1754,#952),#1259,.F.);
#8946=ADVANCED_FACE('',(#1755),#1260,.T.);
#8947=ADVANCED_FACE('',(#1756),#1261,.T.);
#8948=ADVANCED_FACE('',(#1757),#1262,.T.);
#8949=ADVANCED_FACE('',(#1758,#953),#1263,.T.);
#8950=ADVANCED_FACE('',(#1759),#8474,.F.);
#8951=ADVANCED_FACE('',(#1760),#8475,.F.);
#8952=ADVANCED_FACE('',(#1761),#8476,.F.);
#8953=ADVANCED_FACE('',(#1762),#8477,.F.);
#8954=ADVANCED_FACE('',(#1763),#8478,.F.);
#8955=ADVANCED_FACE('',(#1764),#8479,.F.);
#8956=ADVANCED_FACE('',(#1765),#1264,.T.);
#8957=ADVANCED_FACE('',(#1766,#954,#955,#956,#957,#958,#959),#1265,.T.);
#8958=ADVANCED_FACE('',(#1767),#1266,.T.);
#8959=ADVANCED_FACE('',(#1768,#960,#961,#962,#963,#964,#965),#1267,.T.);
#8960=ADVANCED_FACE('',(#1769,#966),#1268,.T.);
#8961=ADVANCED_FACE('',(#1770),#1269,.F.);
#8962=ADVANCED_FACE('',(#1771),#8480,.F.);
#8963=ADVANCED_FACE('',(#1772),#8481,.F.);
#8964=ADVANCED_FACE('',(#1773),#8482,.F.);
#8965=ADVANCED_FACE('',(#1774),#8483,.F.);
#8966=ADVANCED_FACE('',(#1775),#8484,.F.);
#8967=ADVANCED_FACE('',(#1776),#8485,.F.);
#8968=ADVANCED_FACE('',(#1777),#1270,.T.);
#8969=ADVANCED_FACE('',(#1778,#967,#968,#969,#970,#971,#972),#1271,.T.);
#8970=ADVANCED_FACE('',(#1779),#1272,.T.);
#8971=ADVANCED_FACE('',(#1780,#973,#974,#975,#976,#977,#978),#1273,.T.);
#8972=ADVANCED_FACE('',(#1781),#1274,.T.);
#8973=ADVANCED_FACE('',(#1782),#1275,.F.);
#8974=ADVANCED_FACE('',(#1783),#8486,.F.);
#8975=ADVANCED_FACE('',(#1784),#8487,.F.);
#8976=ADVANCED_FACE('',(#1785),#8488,.F.);
#8977=ADVANCED_FACE('',(#1786),#8489,.F.);
#8978=ADVANCED_FACE('',(#1787),#8490,.F.);
#8979=ADVANCED_FACE('',(#1788),#8491,.F.);
#8980=ADVANCED_FACE('',(#1789),#1276,.T.);
#8981=ADVANCED_FACE('',(#1790,#979,#980,#981,#982,#983,#984),#1277,.T.);
#8982=ADVANCED_FACE('',(#1791),#1278,.T.);
#8983=ADVANCED_FACE('',(#1792,#985,#986,#987,#988,#989,#990),#1279,.T.);
#8984=ADVANCED_FACE('',(#1793),#1280,.T.);
#8985=ADVANCED_FACE('',(#1794),#1281,.F.);
#8986=ADVANCED_FACE('',(#1795),#8492,.F.);
#8987=ADVANCED_FACE('',(#1796),#1282,.T.);
#8988=ADVANCED_FACE('',(#1797,#991),#1283,.T.);
#8989=ADVANCED_FACE('',(#1798),#8493,.T.);
#8990=ADVANCED_FACE('',(#1799),#1284,.F.);
#8991=ADVANCED_FACE('',(#1800),#8494,.T.);
#8992=ADVANCED_FACE('',(#1801,#992),#1285,.T.);
#8993=ADVANCED_FACE('',(#1802),#8495,.F.);
#8994=ADVANCED_FACE('',(#1803),#8496,.T.);
#8995=ADVANCED_FACE('',(#1804,#993),#1286,.T.);
#8996=ADVANCED_FACE('',(#1805,#994),#1287,.F.);
#8997=ADVANCED_FACE('',(#1806),#8497,.F.);
#8998=ADVANCED_FACE('',(#1807),#8498,.T.);
#8999=ADVANCED_FACE('',(#1808,#995),#1288,.T.);
#9000=ADVANCED_FACE('',(#1809,#996),#1289,.F.);
#9001=ADVANCED_FACE('',(#1810),#8499,.F.);
#9002=ADVANCED_FACE('',(#1811),#8500,.T.);
#9003=ADVANCED_FACE('',(#1812,#997),#1290,.T.);
#9004=ADVANCED_FACE('',(#1813,#998),#1291,.F.);
#9005=ADVANCED_FACE('',(#1814),#1292,.F.);
#9006=ADVANCED_FACE('',(#1815),#1293,.F.);
#9007=ADVANCED_FACE('',(#1816),#1294,.F.);
#9008=ADVANCED_FACE('',(#1817),#1295,.F.);
#9009=ADVANCED_FACE('',(#1818),#1296,.F.);
#9010=ADVANCED_FACE('',(#1819,#999),#1297,.T.);
#9011=ADVANCED_FACE('',(#1820),#8501,.T.);
#9012=ADVANCED_FACE('',(#1821,#1000),#1298,.T.);
#9013=ADVANCED_FACE('',(#1822),#8502,.T.);
#9014=ADVANCED_FACE('',(#1823,#1001),#1299,.T.);
#9015=ADVANCED_FACE('',(#1824),#8503,.T.);
#9016=ADVANCED_FACE('',(#1825,#1002),#1300,.T.);
#9017=ADVANCED_FACE('',(#1826),#8504,.T.);
#9018=ADVANCED_FACE('',(#1827,#1003),#1301,.T.);
#9019=ADVANCED_FACE('',(#1828),#8505,.T.);
#9020=ADVANCED_FACE('',(#1829,#1004),#1302,.T.);
#9021=ADVANCED_FACE('',(#1830,#1005),#8506,.F.);
#9022=ADVANCED_FACE('',(#1831),#1303,.F.);
#9023=ADVANCED_FACE('',(#1832),#1304,.F.);
#9024=ADVANCED_FACE('',(#1833),#1305,.F.);
#9025=ADVANCED_FACE('',(#1834),#1306,.F.);
#9026=ADVANCED_FACE('',(#1835,#1006),#1307,.T.);
#9027=ADVANCED_FACE('',(#1836,#1007),#8507,.T.);
#9028=ADVANCED_FACE('',(#1837,#1008),#1308,.T.);
#9029=ADVANCED_FACE('',(#1838,#1009),#8508,.F.);
#9030=ADVANCED_FACE('',(#1839),#1309,.F.);
#9031=ADVANCED_FACE('',(#1840),#1310,.F.);
#9032=ADVANCED_FACE('',(#1841),#1311,.F.);
#9033=ADVANCED_FACE('',(#1842),#1312,.F.);
#9034=ADVANCED_FACE('',(#1843),#1313,.F.);
#9035=ADVANCED_FACE('',(#1844),#1314,.F.);
#9036=ADVANCED_FACE('',(#1845),#1315,.F.);
#9037=ADVANCED_FACE('',(#1846),#1316,.F.);
#9038=ADVANCED_FACE('',(#1847),#1317,.F.);
#9039=ADVANCED_FACE('',(#1848),#1318,.T.);
#9040=ADVANCED_FACE('',(#1849),#556,.T.);
#9041=ADVANCED_FACE('',(#1850),#8509,.T.);
#9042=ADVANCED_FACE('',(#1851),#557,.T.);
#9043=ADVANCED_FACE('',(#1852,#1010),#1319,.T.);
#9044=ADVANCED_FACE('',(#1853),#558,.T.);
#9045=ADVANCED_FACE('',(#1854),#8510,.T.);
#9046=CLOSED_SHELL('',(#8511,#8512,#8513,#8514,#8515,#8516,#8517,#8518,
#8519,#8520,#8521,#8522,#8523,#8524,#8525,#8526,#8527,#8528));
#9047=CLOSED_SHELL('',(#8529,#8530,#8531,#8532,#8533,#8534,#8535,#8536,
#8537,#8538,#8539,#8540,#8541,#8542,#8543,#8544,#8545,#8546,#8547,#8548,
#8549,#8550));
#9048=CLOSED_SHELL('',(#8551,#8552,#8553,#8554));
#9049=CLOSED_SHELL('',(#8555,#8556,#8557,#8558));
#9050=CLOSED_SHELL('',(#8559,#8560,#8561,#8562,#8563,#8564,#8565,#8566,
#8567,#8568,#8569,#8570,#8571,#8572,#8573,#8574,#8575,#8576,#8577,#8578,
#8579,#8580));
#9051=CLOSED_SHELL('',(#8581,#8582,#8583,#8584));
#9052=CLOSED_SHELL('',(#8585,#8586,#8587,#8588));
#9053=CLOSED_SHELL('',(#8589,#8590,#8591,#8592,#8593,#8594,#8595,#8596,
#8597,#8598,#8599,#8600,#8601,#8602,#8603,#8604,#8605,#8606,#8607,#8608,
#8609));
#9054=CLOSED_SHELL('',(#8610,#8611,#8612,#8613,#8614,#8615,#8616,#8617,
#8618,#8619,#8620,#8621,#8622,#8623,#8624,#8625,#8626,#8627,#8628,#8629,
#8630));
#9055=CLOSED_SHELL('',(#8631,#8632,#8633,#8634,#8635,#8636));
#9056=CLOSED_SHELL('',(#8637,#8638,#8639,#8640,#8641,#8642));
#9057=CLOSED_SHELL('',(#8643,#8644,#8645,#8646,#8647,#8648,#8649,#8650,
#8651));
#9058=CLOSED_SHELL('',(#8652,#8653,#8654,#8655,#8656,#8657,#8658,#8659));
#9059=CLOSED_SHELL('',(#8660,#8661,#8662,#8663,#8664,#8665,#8666,#8667,
#8668,#8669,#8670,#8671,#8672,#8673,#8674,#8675,#8676,#8677,#8678,#8679,
#8680,#8681,#8682,#8683,#8684));
#9060=CLOSED_SHELL('',(#8685,#8686,#8687,#8688));
#9061=CLOSED_SHELL('',(#8689,#8690,#8691,#8692,#8693,#8694,#8695,#8696,
#8697,#8698,#8699,#8700));
#9062=CLOSED_SHELL('',(#8701,#8702,#8703,#8704));
#9063=CLOSED_SHELL('',(#8705,#8706,#8707,#8708,#8709,#8710,#8711,#8712));
#9064=CLOSED_SHELL('',(#8713,#8714,#8715,#8716,#8717,#8718,#8719,#8720));
#9065=CLOSED_SHELL('',(#8721,#8722,#8723,#8724,#8725,#8726,#8727,#8728,
#8729,#8730,#8731,#8732,#8733,#8734,#8735,#8736,#8737,#8738,#8739,#8740,
#8741,#8742,#8743));
#9066=CLOSED_SHELL('',(#8744,#8745,#8746,#8747,#8748));
#9067=CLOSED_SHELL('',(#8749,#8750,#8751,#8752,#8753,#8754,#8755,#8756));
#9068=CLOSED_SHELL('',(#8757,#8758,#8759,#8760,#8761,#8762,#8763,#8764));
#9069=CLOSED_SHELL('',(#8765,#8766,#8767,#8768,#8769,#8770,#8771,#8772,
#8773));
#9070=CLOSED_SHELL('',(#8774,#8775,#8776,#8777,#8778,#8779,#8780,#8781));
#9071=CLOSED_SHELL('',(#8782,#8783,#8784,#8785));
#9072=CLOSED_SHELL('',(#8786,#8787,#8788,#8789,#8790,#8791,#8792));
#9073=CLOSED_SHELL('',(#8793,#8794,#8795,#8796,#8797,#8798,#8799));
#9074=CLOSED_SHELL('',(#8800,#8801,#8802,#8803,#8804,#8805,#8806));
#9075=CLOSED_SHELL('',(#8807,#8808,#8809,#8810));
#9076=CLOSED_SHELL('',(#8811,#8812,#8813,#8814,#8815,#8816,#8817,#8818,
#8819,#8820,#8821,#8822,#8823,#8824,#8825,#8826,#8827));
#9077=CLOSED_SHELL('',(#8828,#8829,#8830,#8831,#8832,#8833,#8834));
#9078=CLOSED_SHELL('',(#8835,#8836,#8837,#8838));
#9079=CLOSED_SHELL('',(#8839,#8840,#8841,#8842));
#9080=CLOSED_SHELL('',(#8843,#8844,#8845,#8846));
#9081=CLOSED_SHELL('',(#8847,#8848,#8849,#8850,#8851,#8852,#8853,#8854,
#8855,#8856));
#9082=CLOSED_SHELL('',(#8857,#8858,#8859,#8860,#8861,#8862,#8863,#8864,
#8865,#8866,#8867,#8868));
#9083=CLOSED_SHELL('',(#8869,#8870,#8871,#8872,#8873,#8874,#8875,#8876));
#9084=CLOSED_SHELL('',(#8877,#8878,#8879,#8880));
#9085=CLOSED_SHELL('',(#8881,#8882,#8883,#8884));
#9086=CLOSED_SHELL('',(#8885,#8886,#8887,#8888));
#9087=CLOSED_SHELL('',(#8889,#8890,#8891,#8892));
#9088=CLOSED_SHELL('',(#8893,#8894,#8895,#8896,#8897,#8898,#8899,#8900));
#9089=CLOSED_SHELL('',(#8901,#8902,#8903,#8904,#8905,#8906,#8907,#8908));
#9090=CLOSED_SHELL('',(#8909));
#9091=CLOSED_SHELL('',(#8910));
#9092=CLOSED_SHELL('',(#8911));
#9093=CLOSED_SHELL('',(#8912));
#9094=CLOSED_SHELL('',(#8913));
#9095=CLOSED_SHELL('',(#8914));
#9096=CLOSED_SHELL('',(#8915));
#9097=CLOSED_SHELL('',(#8916));
#9098=CLOSED_SHELL('',(#8917,#8918,#8919,#8920,#8921,#8922,#8923,#8924,
#8925,#8926,#8927,#8928,#8929,#8930,#8931,#8932,#8933,#8934,#8935));
#9099=CLOSED_SHELL('',(#8936,#8937,#8938,#8939));
#9100=CLOSED_SHELL('',(#8940,#8941,#8942,#8943));
#9101=CLOSED_SHELL('',(#8944,#8945,#8946,#8947,#8948,#8949,#8950,#8951,
#8952,#8953,#8954,#8955,#8956,#8957,#8958,#8959,#8960,#8961));
#9102=CLOSED_SHELL('',(#8962,#8963,#8964,#8965,#8966,#8967,#8968,#8969,
#8970,#8971,#8972,#8973));
#9103=CLOSED_SHELL('',(#8974,#8975,#8976,#8977,#8978,#8979,#8980,#8981,
#8982,#8983,#8984,#8985));
#9104=CLOSED_SHELL('',(#8986,#8987,#8988,#8989,#8990,#8991,#8992));
#9105=CLOSED_SHELL('',(#8993,#8994,#8995,#8996));
#9106=CLOSED_SHELL('',(#8997,#8998,#8999,#9000));
#9107=CLOSED_SHELL('',(#9001,#9002,#9003,#9004));
#9108=CLOSED_SHELL('',(#9005,#9006,#9007,#9008,#9009,#9010,#9011,#9012,
#9013,#9014,#9015,#9016,#9017,#9018,#9019,#9020,#9021));
#9109=CLOSED_SHELL('',(#9022,#9023,#9024,#9025,#9026,#9027,#9028,#9029));
#9110=CLOSED_SHELL('',(#9030,#9031,#9032,#9033,#9034,#9035,#9036,#9037));
#9111=CLOSED_SHELL('',(#9038,#9039,#9040,#9041,#9042,#9043,#9044,#9045));
#9112=DERIVED_UNIT_ELEMENT(#9216,1.);
#9113=DERIVED_UNIT_ELEMENT(#17324,-3.);
#9114=DERIVED_UNIT_ELEMENT(#9216,1.);
#9115=DERIVED_UNIT_ELEMENT(#17324,-3.);
#9116=DERIVED_UNIT_ELEMENT(#9216,1.);
#9117=DERIVED_UNIT_ELEMENT(#17324,-3.);
#9118=DERIVED_UNIT_ELEMENT(#9216,1.);
#9119=DERIVED_UNIT_ELEMENT(#17324,-3.);
#9120=DERIVED_UNIT_ELEMENT(#9216,1.);
#9121=DERIVED_UNIT_ELEMENT(#17324,-3.);
#9122=DERIVED_UNIT_ELEMENT(#9216,1.);
#9123=DERIVED_UNIT_ELEMENT(#17324,-3.);
#9124=DERIVED_UNIT_ELEMENT(#9216,1.);
#9125=DERIVED_UNIT_ELEMENT(#17324,-3.);
#9126=DERIVED_UNIT_ELEMENT(#9216,1.);
#9127=DERIVED_UNIT_ELEMENT(#17324,-3.);
#9128=DERIVED_UNIT_ELEMENT(#9216,1.);
#9129=DERIVED_UNIT_ELEMENT(#17324,-3.);
#9130=DERIVED_UNIT_ELEMENT(#9216,1.);
#9131=DERIVED_UNIT_ELEMENT(#17324,-3.);
#9132=DERIVED_UNIT_ELEMENT(#9216,1.);
#9133=DERIVED_UNIT_ELEMENT(#17324,-3.);
#9134=DERIVED_UNIT_ELEMENT(#9216,1.);
#9135=DERIVED_UNIT_ELEMENT(#17324,-3.);
#9136=DERIVED_UNIT_ELEMENT(#9216,1.);
#9137=DERIVED_UNIT_ELEMENT(#17324,-3.);
#9138=DERIVED_UNIT_ELEMENT(#9216,1.);
#9139=DERIVED_UNIT_ELEMENT(#17324,-3.);
#9140=DERIVED_UNIT_ELEMENT(#9216,1.);
#9141=DERIVED_UNIT_ELEMENT(#17324,-3.);
#9142=DERIVED_UNIT_ELEMENT(#9216,1.);
#9143=DERIVED_UNIT_ELEMENT(#17324,-3.);
#9144=DERIVED_UNIT_ELEMENT(#9216,1.);
#9145=DERIVED_UNIT_ELEMENT(#17324,-3.);
#9146=DERIVED_UNIT_ELEMENT(#9216,1.);
#9147=DERIVED_UNIT_ELEMENT(#17324,-3.);
#9148=DERIVED_UNIT_ELEMENT(#9216,1.);
#9149=DERIVED_UNIT_ELEMENT(#17324,-3.);
#9150=DERIVED_UNIT_ELEMENT(#9216,1.);
#9151=DERIVED_UNIT_ELEMENT(#17324,-3.);
#9152=DERIVED_UNIT_ELEMENT(#9216,1.);
#9153=DERIVED_UNIT_ELEMENT(#17324,-3.);
#9154=DERIVED_UNIT_ELEMENT(#9216,1.);
#9155=DERIVED_UNIT_ELEMENT(#17324,-3.);
#9156=DERIVED_UNIT_ELEMENT(#9216,1.);
#9157=DERIVED_UNIT_ELEMENT(#17324,-3.);
#9158=DERIVED_UNIT_ELEMENT(#9216,1.);
#9159=DERIVED_UNIT_ELEMENT(#17324,-3.);
#9160=DERIVED_UNIT_ELEMENT(#9216,1.);
#9161=DERIVED_UNIT_ELEMENT(#17324,-3.);
#9162=DERIVED_UNIT_ELEMENT(#9216,1.);
#9163=DERIVED_UNIT_ELEMENT(#17324,-3.);
#9164=DERIVED_UNIT_ELEMENT(#9216,1.);
#9165=DERIVED_UNIT_ELEMENT(#17324,-3.);
#9166=DERIVED_UNIT_ELEMENT(#9216,1.);
#9167=DERIVED_UNIT_ELEMENT(#17324,-3.);
#9168=DERIVED_UNIT_ELEMENT(#9216,1.);
#9169=DERIVED_UNIT_ELEMENT(#17324,-3.);
#9170=DERIVED_UNIT_ELEMENT(#9216,1.);
#9171=DERIVED_UNIT_ELEMENT(#17324,-3.);
#9172=DERIVED_UNIT_ELEMENT(#9216,1.);
#9173=DERIVED_UNIT_ELEMENT(#17324,-3.);
#9174=DERIVED_UNIT_ELEMENT(#9216,1.);
#9175=DERIVED_UNIT_ELEMENT(#17324,-3.);
#9176=DERIVED_UNIT_ELEMENT(#9216,1.);
#9177=DERIVED_UNIT_ELEMENT(#17324,-3.);
#9178=DERIVED_UNIT_ELEMENT(#9216,1.);
#9179=DERIVED_UNIT_ELEMENT(#17324,-3.);
#9180=DERIVED_UNIT_ELEMENT(#9216,1.);
#9181=DERIVED_UNIT_ELEMENT(#17324,-3.);
#9182=DERIVED_UNIT_ELEMENT(#9216,1.);
#9183=DERIVED_UNIT_ELEMENT(#17324,-3.);
#9184=DERIVED_UNIT_ELEMENT(#9216,1.);
#9185=DERIVED_UNIT_ELEMENT(#17324,-3.);
#9186=DERIVED_UNIT_ELEMENT(#9216,1.);
#9187=DERIVED_UNIT_ELEMENT(#17324,-3.);
#9188=DERIVED_UNIT_ELEMENT(#9216,1.);
#9189=DERIVED_UNIT_ELEMENT(#17324,-3.);
#9190=DERIVED_UNIT_ELEMENT(#9216,1.);
#9191=DERIVED_UNIT_ELEMENT(#17324,-3.);
#9192=DERIVED_UNIT_ELEMENT(#9216,1.);
#9193=DERIVED_UNIT_ELEMENT(#17324,-3.);
#9194=DERIVED_UNIT_ELEMENT(#9216,1.);
#9195=DERIVED_UNIT_ELEMENT(#17324,-3.);
#9196=DERIVED_UNIT_ELEMENT(#9216,1.);
#9197=DERIVED_UNIT_ELEMENT(#17324,-3.);
#9198=DERIVED_UNIT_ELEMENT(#9216,1.);
#9199=DERIVED_UNIT_ELEMENT(#17324,-3.);
#9200=DERIVED_UNIT_ELEMENT(#9216,1.);
#9201=DERIVED_UNIT_ELEMENT(#17324,-3.);
#9202=DERIVED_UNIT_ELEMENT(#9216,1.);
#9203=DERIVED_UNIT_ELEMENT(#17324,-3.);
#9204=DERIVED_UNIT_ELEMENT(#9216,1.);
#9205=DERIVED_UNIT_ELEMENT(#17324,-3.);
#9206=DERIVED_UNIT_ELEMENT(#9216,1.);
#9207=DERIVED_UNIT_ELEMENT(#17324,-3.);
#9208=DERIVED_UNIT_ELEMENT(#9216,1.);
#9209=DERIVED_UNIT_ELEMENT(#17324,-3.);
#9210=DERIVED_UNIT_ELEMENT(#9216,1.);
#9211=DERIVED_UNIT_ELEMENT(#17324,-3.);
#9212=DERIVED_UNIT_ELEMENT(#9216,1.);
#9213=DERIVED_UNIT_ELEMENT(#17324,-3.);
#9214=DERIVED_UNIT_ELEMENT(#9216,1.);
#9215=DERIVED_UNIT_ELEMENT(#17324,-3.);
#9216=(
MASS_UNIT()
NAMED_UNIT(*)
SI_UNIT(.KILO.,.GRAM.)
);
#9217=DERIVED_UNIT((#9112,#9113));
#9218=DERIVED_UNIT((#9114,#9115));
#9219=DERIVED_UNIT((#9116,#9117));
#9220=DERIVED_UNIT((#9118,#9119));
#9221=DERIVED_UNIT((#9120,#9121));
#9222=DERIVED_UNIT((#9122,#9123));
#9223=DERIVED_UNIT((#9124,#9125));
#9224=DERIVED_UNIT((#9126,#9127));
#9225=DERIVED_UNIT((#9128,#9129));
#9226=DERIVED_UNIT((#9130,#9131));
#9227=DERIVED_UNIT((#9132,#9133));
#9228=DERIVED_UNIT((#9134,#9135));
#9229=DERIVED_UNIT((#9136,#9137));
#9230=DERIVED_UNIT((#9138,#9139));
#9231=DERIVED_UNIT((#9140,#9141));
#9232=DERIVED_UNIT((#9142,#9143));
#9233=DERIVED_UNIT((#9144,#9145));
#9234=DERIVED_UNIT((#9146,#9147));
#9235=DERIVED_UNIT((#9148,#9149));
#9236=DERIVED_UNIT((#9150,#9151));
#9237=DERIVED_UNIT((#9152,#9153));
#9238=DERIVED_UNIT((#9154,#9155));
#9239=DERIVED_UNIT((#9156,#9157));
#9240=DERIVED_UNIT((#9158,#9159));
#9241=DERIVED_UNIT((#9160,#9161));
#9242=DERIVED_UNIT((#9162,#9163));
#9243=DERIVED_UNIT((#9164,#9165));
#9244=DERIVED_UNIT((#9166,#9167));
#9245=DERIVED_UNIT((#9168,#9169));
#9246=DERIVED_UNIT((#9170,#9171));
#9247=DERIVED_UNIT((#9172,#9173));
#9248=DERIVED_UNIT((#9174,#9175));
#9249=DERIVED_UNIT((#9176,#9177));
#9250=DERIVED_UNIT((#9178,#9179));
#9251=DERIVED_UNIT((#9180,#9181));
#9252=DERIVED_UNIT((#9182,#9183));
#9253=DERIVED_UNIT((#9184,#9185));
#9254=DERIVED_UNIT((#9186,#9187));
#9255=DERIVED_UNIT((#9188,#9189));
#9256=DERIVED_UNIT((#9190,#9191));
#9257=DERIVED_UNIT((#9192,#9193));
#9258=DERIVED_UNIT((#9194,#9195));
#9259=DERIVED_UNIT((#9196,#9197));
#9260=DERIVED_UNIT((#9198,#9199));
#9261=DERIVED_UNIT((#9200,#9201));
#9262=DERIVED_UNIT((#9202,#9203));
#9263=DERIVED_UNIT((#9204,#9205));
#9264=DERIVED_UNIT((#9206,#9207));
#9265=DERIVED_UNIT((#9208,#9209));
#9266=DERIVED_UNIT((#9210,#9211));
#9267=DERIVED_UNIT((#9212,#9213));
#9268=DERIVED_UNIT((#9214,#9215));
#9269=MEASURE_REPRESENTATION_ITEM('density measure',
POSITIVE_RATIO_MEASURE(7850.),#9217);
#9270=MEASURE_REPRESENTATION_ITEM('density measure',
POSITIVE_RATIO_MEASURE(7850.),#9218);
#9271=MEASURE_REPRESENTATION_ITEM('density measure',
POSITIVE_RATIO_MEASURE(7850.),#9219);
#9272=MEASURE_REPRESENTATION_ITEM('density measure',
POSITIVE_RATIO_MEASURE(7850.),#9220);
#9273=MEASURE_REPRESENTATION_ITEM('density measure',
POSITIVE_RATIO_MEASURE(7850.),#9221);
#9274=MEASURE_REPRESENTATION_ITEM('density measure',
POSITIVE_RATIO_MEASURE(7850.),#9222);
#9275=MEASURE_REPRESENTATION_ITEM('density measure',
POSITIVE_RATIO_MEASURE(7850.),#9223);
#9276=MEASURE_REPRESENTATION_ITEM('density measure',
POSITIVE_RATIO_MEASURE(7850.),#9224);
#9277=MEASURE_REPRESENTATION_ITEM('density measure',
POSITIVE_RATIO_MEASURE(7850.),#9225);
#9278=MEASURE_REPRESENTATION_ITEM('density measure',
POSITIVE_RATIO_MEASURE(7850.),#9226);
#9279=MEASURE_REPRESENTATION_ITEM('density measure',
POSITIVE_RATIO_MEASURE(7850.),#9227);
#9280=MEASURE_REPRESENTATION_ITEM('density measure',
POSITIVE_RATIO_MEASURE(7850.),#9228);
#9281=MEASURE_REPRESENTATION_ITEM('density measure',
POSITIVE_RATIO_MEASURE(7850.),#9229);
#9282=MEASURE_REPRESENTATION_ITEM('density measure',
POSITIVE_RATIO_MEASURE(7850.),#9230);
#9283=MEASURE_REPRESENTATION_ITEM('density measure',
POSITIVE_RATIO_MEASURE(7850.),#9231);
#9284=MEASURE_REPRESENTATION_ITEM('density measure',
POSITIVE_RATIO_MEASURE(7850.),#9232);
#9285=MEASURE_REPRESENTATION_ITEM('density measure',
POSITIVE_RATIO_MEASURE(7850.),#9233);
#9286=MEASURE_REPRESENTATION_ITEM('density measure',
POSITIVE_RATIO_MEASURE(7850.),#9234);
#9287=MEASURE_REPRESENTATION_ITEM('density measure',
POSITIVE_RATIO_MEASURE(7850.),#9235);
#9288=MEASURE_REPRESENTATION_ITEM('density measure',
POSITIVE_RATIO_MEASURE(7850.),#9236);
#9289=MEASURE_REPRESENTATION_ITEM('density measure',
POSITIVE_RATIO_MEASURE(7850.),#9237);
#9290=MEASURE_REPRESENTATION_ITEM('density measure',
POSITIVE_RATIO_MEASURE(7850.),#9238);
#9291=MEASURE_REPRESENTATION_ITEM('density measure',
POSITIVE_RATIO_MEASURE(7850.),#9239);
#9292=MEASURE_REPRESENTATION_ITEM('density measure',
POSITIVE_RATIO_MEASURE(7850.),#9240);
#9293=MEASURE_REPRESENTATION_ITEM('density measure',
POSITIVE_RATIO_MEASURE(7850.),#9241);
#9294=MEASURE_REPRESENTATION_ITEM('density measure',
POSITIVE_RATIO_MEASURE(7850.),#9242);
#9295=MEASURE_REPRESENTATION_ITEM('density measure',
POSITIVE_RATIO_MEASURE(7850.),#9243);
#9296=MEASURE_REPRESENTATION_ITEM('density measure',
POSITIVE_RATIO_MEASURE(7850.),#9244);
#9297=MEASURE_REPRESENTATION_ITEM('density measure',
POSITIVE_RATIO_MEASURE(7850.),#9245);
#9298=MEASURE_REPRESENTATION_ITEM('density measure',
POSITIVE_RATIO_MEASURE(7850.),#9246);
#9299=MEASURE_REPRESENTATION_ITEM('density measure',
POSITIVE_RATIO_MEASURE(7850.),#9247);
#9300=MEASURE_REPRESENTATION_ITEM('density measure',
POSITIVE_RATIO_MEASURE(7850.),#9248);
#9301=MEASURE_REPRESENTATION_ITEM('density measure',
POSITIVE_RATIO_MEASURE(7850.),#9249);
#9302=MEASURE_REPRESENTATION_ITEM('density measure',
POSITIVE_RATIO_MEASURE(7850.),#9250);
#9303=MEASURE_REPRESENTATION_ITEM('density measure',
POSITIVE_RATIO_MEASURE(7850.),#9251);
#9304=MEASURE_REPRESENTATION_ITEM('density measure',
POSITIVE_RATIO_MEASURE(7850.),#9252);
#9305=MEASURE_REPRESENTATION_ITEM('density measure',
POSITIVE_RATIO_MEASURE(7850.),#9253);
#9306=MEASURE_REPRESENTATION_ITEM('density measure',
POSITIVE_RATIO_MEASURE(7850.),#9254);
#9307=MEASURE_REPRESENTATION_ITEM('density measure',
POSITIVE_RATIO_MEASURE(7850.),#9255);
#9308=MEASURE_REPRESENTATION_ITEM('density measure',
POSITIVE_RATIO_MEASURE(7850.),#9256);
#9309=MEASURE_REPRESENTATION_ITEM('density measure',
POSITIVE_RATIO_MEASURE(7850.),#9257);
#9310=MEASURE_REPRESENTATION_ITEM('density measure',
POSITIVE_RATIO_MEASURE(7850.),#9258);
#9311=MEASURE_REPRESENTATION_ITEM('density measure',
POSITIVE_RATIO_MEASURE(7850.),#9259);
#9312=MEASURE_REPRESENTATION_ITEM('density measure',
POSITIVE_RATIO_MEASURE(7850.),#9260);
#9313=MEASURE_REPRESENTATION_ITEM('density measure',
POSITIVE_RATIO_MEASURE(7850.),#9261);
#9314=MEASURE_REPRESENTATION_ITEM('density measure',
POSITIVE_RATIO_MEASURE(7850.),#9262);
#9315=MEASURE_REPRESENTATION_ITEM('density measure',
POSITIVE_RATIO_MEASURE(7850.),#9263);
#9316=MEASURE_REPRESENTATION_ITEM('density measure',
POSITIVE_RATIO_MEASURE(7850.),#9264);
#9317=MEASURE_REPRESENTATION_ITEM('density measure',
POSITIVE_RATIO_MEASURE(7850.),#9265);
#9318=MEASURE_REPRESENTATION_ITEM('density measure',
POSITIVE_RATIO_MEASURE(7850.),#9266);
#9319=MEASURE_REPRESENTATION_ITEM('density measure',
POSITIVE_RATIO_MEASURE(7850.),#9267);
#9320=MEASURE_REPRESENTATION_ITEM('density measure',
POSITIVE_RATIO_MEASURE(7850.),#9268);
#9321=PROPERTY_DEFINITION_REPRESENTATION(#9581,#9425);
#9322=PROPERTY_DEFINITION_REPRESENTATION(#9582,#9426);
#9323=PROPERTY_DEFINITION_REPRESENTATION(#9583,#9427);
#9324=PROPERTY_DEFINITION_REPRESENTATION(#9584,#9428);
#9325=PROPERTY_DEFINITION_REPRESENTATION(#9585,#9429);
#9326=PROPERTY_DEFINITION_REPRESENTATION(#9586,#9430);
#9327=PROPERTY_DEFINITION_REPRESENTATION(#9587,#9431);
#9328=PROPERTY_DEFINITION_REPRESENTATION(#9588,#9432);
#9329=PROPERTY_DEFINITION_REPRESENTATION(#9589,#9433);
#9330=PROPERTY_DEFINITION_REPRESENTATION(#9590,#9434);
#9331=PROPERTY_DEFINITION_REPRESENTATION(#9591,#9435);
#9332=PROPERTY_DEFINITION_REPRESENTATION(#9592,#9436);
#9333=PROPERTY_DEFINITION_REPRESENTATION(#9593,#9437);
#9334=PROPERTY_DEFINITION_REPRESENTATION(#9594,#9438);
#9335=PROPERTY_DEFINITION_REPRESENTATION(#9595,#9439);
#9336=PROPERTY_DEFINITION_REPRESENTATION(#9596,#9440);
#9337=PROPERTY_DEFINITION_REPRESENTATION(#9597,#9441);
#9338=PROPERTY_DEFINITION_REPRESENTATION(#9598,#9442);
#9339=PROPERTY_DEFINITION_REPRESENTATION(#9599,#9443);
#9340=PROPERTY_DEFINITION_REPRESENTATION(#9600,#9444);
#9341=PROPERTY_DEFINITION_REPRESENTATION(#9601,#9445);
#9342=PROPERTY_DEFINITION_REPRESENTATION(#9602,#9446);
#9343=PROPERTY_DEFINITION_REPRESENTATION(#9603,#9447);
#9344=PROPERTY_DEFINITION_REPRESENTATION(#9604,#9448);
#9345=PROPERTY_DEFINITION_REPRESENTATION(#9605,#9449);
#9346=PROPERTY_DEFINITION_REPRESENTATION(#9606,#9450);
#9347=PROPERTY_DEFINITION_REPRESENTATION(#9607,#9451);
#9348=PROPERTY_DEFINITION_REPRESENTATION(#9608,#9452);
#9349=PROPERTY_DEFINITION_REPRESENTATION(#9609,#9453);
#9350=PROPERTY_DEFINITION_REPRESENTATION(#9610,#9454);
#9351=PROPERTY_DEFINITION_REPRESENTATION(#9611,#9455);
#9352=PROPERTY_DEFINITION_REPRESENTATION(#9612,#9456);
#9353=PROPERTY_DEFINITION_REPRESENTATION(#9613,#9457);
#9354=PROPERTY_DEFINITION_REPRESENTATION(#9614,#9458);
#9355=PROPERTY_DEFINITION_REPRESENTATION(#9615,#9459);
#9356=PROPERTY_DEFINITION_REPRESENTATION(#9616,#9460);
#9357=PROPERTY_DEFINITION_REPRESENTATION(#9617,#9461);
#9358=PROPERTY_DEFINITION_REPRESENTATION(#9618,#9462);
#9359=PROPERTY_DEFINITION_REPRESENTATION(#9619,#9463);
#9360=PROPERTY_DEFINITION_REPRESENTATION(#9620,#9464);
#9361=PROPERTY_DEFINITION_REPRESENTATION(#9621,#9465);
#9362=PROPERTY_DEFINITION_REPRESENTATION(#9622,#9466);
#9363=PROPERTY_DEFINITION_REPRESENTATION(#9623,#9467);
#9364=PROPERTY_DEFINITION_REPRESENTATION(#9624,#9468);
#9365=PROPERTY_DEFINITION_REPRESENTATION(#9625,#9469);
#9366=PROPERTY_DEFINITION_REPRESENTATION(#9626,#9470);
#9367=PROPERTY_DEFINITION_REPRESENTATION(#9627,#9471);
#9368=PROPERTY_DEFINITION_REPRESENTATION(#9628,#9472);
#9369=PROPERTY_DEFINITION_REPRESENTATION(#9629,#9473);
#9370=PROPERTY_DEFINITION_REPRESENTATION(#9630,#9474);
#9371=PROPERTY_DEFINITION_REPRESENTATION(#9631,#9475);
#9372=PROPERTY_DEFINITION_REPRESENTATION(#9632,#9476);
#9373=PROPERTY_DEFINITION_REPRESENTATION(#9633,#9477);
#9374=PROPERTY_DEFINITION_REPRESENTATION(#9634,#9478);
#9375=PROPERTY_DEFINITION_REPRESENTATION(#9635,#9479);
#9376=PROPERTY_DEFINITION_REPRESENTATION(#9636,#9480);
#9377=PROPERTY_DEFINITION_REPRESENTATION(#9637,#9481);
#9378=PROPERTY_DEFINITION_REPRESENTATION(#9638,#9482);
#9379=PROPERTY_DEFINITION_REPRESENTATION(#9639,#9483);
#9380=PROPERTY_DEFINITION_REPRESENTATION(#9640,#9484);
#9381=PROPERTY_DEFINITION_REPRESENTATION(#9641,#9485);
#9382=PROPERTY_DEFINITION_REPRESENTATION(#9642,#9486);
#9383=PROPERTY_DEFINITION_REPRESENTATION(#9643,#9487);
#9384=PROPERTY_DEFINITION_REPRESENTATION(#9644,#9488);
#9385=PROPERTY_DEFINITION_REPRESENTATION(#9645,#9489);
#9386=PROPERTY_DEFINITION_REPRESENTATION(#9646,#9490);
#9387=PROPERTY_DEFINITION_REPRESENTATION(#9647,#9491);
#9388=PROPERTY_DEFINITION_REPRESENTATION(#9648,#9492);
#9389=PROPERTY_DEFINITION_REPRESENTATION(#9649,#9493);
#9390=PROPERTY_DEFINITION_REPRESENTATION(#9650,#9494);
#9391=PROPERTY_DEFINITION_REPRESENTATION(#9651,#9495);
#9392=PROPERTY_DEFINITION_REPRESENTATION(#9652,#9496);
#9393=PROPERTY_DEFINITION_REPRESENTATION(#9653,#9497);
#9394=PROPERTY_DEFINITION_REPRESENTATION(#9654,#9498);
#9395=PROPERTY_DEFINITION_REPRESENTATION(#9655,#9499);
#9396=PROPERTY_DEFINITION_REPRESENTATION(#9656,#9500);
#9397=PROPERTY_DEFINITION_REPRESENTATION(#9657,#9501);
#9398=PROPERTY_DEFINITION_REPRESENTATION(#9658,#9502);
#9399=PROPERTY_DEFINITION_REPRESENTATION(#9659,#9503);
#9400=PROPERTY_DEFINITION_REPRESENTATION(#9660,#9504);
#9401=PROPERTY_DEFINITION_REPRESENTATION(#9661,#9505);
#9402=PROPERTY_DEFINITION_REPRESENTATION(#9662,#9506);
#9403=PROPERTY_DEFINITION_REPRESENTATION(#9663,#9507);
#9404=PROPERTY_DEFINITION_REPRESENTATION(#9664,#9508);
#9405=PROPERTY_DEFINITION_REPRESENTATION(#9665,#9509);
#9406=PROPERTY_DEFINITION_REPRESENTATION(#9666,#9510);
#9407=PROPERTY_DEFINITION_REPRESENTATION(#9667,#9511);
#9408=PROPERTY_DEFINITION_REPRESENTATION(#9668,#9512);
#9409=PROPERTY_DEFINITION_REPRESENTATION(#9669,#9513);
#9410=PROPERTY_DEFINITION_REPRESENTATION(#9670,#9514);
#9411=PROPERTY_DEFINITION_REPRESENTATION(#9671,#9515);
#9412=PROPERTY_DEFINITION_REPRESENTATION(#9672,#9516);
#9413=PROPERTY_DEFINITION_REPRESENTATION(#9673,#9517);
#9414=PROPERTY_DEFINITION_REPRESENTATION(#9674,#9518);
#9415=PROPERTY_DEFINITION_REPRESENTATION(#9675,#9519);
#9416=PROPERTY_DEFINITION_REPRESENTATION(#9676,#9520);
#9417=PROPERTY_DEFINITION_REPRESENTATION(#9677,#9521);
#9418=PROPERTY_DEFINITION_REPRESENTATION(#9678,#9522);
#9419=PROPERTY_DEFINITION_REPRESENTATION(#9679,#9523);
#9420=PROPERTY_DEFINITION_REPRESENTATION(#9680,#9524);
#9421=PROPERTY_DEFINITION_REPRESENTATION(#9681,#9525);
#9422=PROPERTY_DEFINITION_REPRESENTATION(#9682,#9526);
#9423=PROPERTY_DEFINITION_REPRESENTATION(#9683,#9527);
#9424=PROPERTY_DEFINITION_REPRESENTATION(#9684,#9528);
#9425=REPRESENTATION('material name',(#9529),#17264);
#9426=REPRESENTATION('density',(#9269),#17264);
#9427=REPRESENTATION('material name',(#9530),#17265);
#9428=REPRESENTATION('density',(#9270),#17265);
#9429=REPRESENTATION('material name',(#9531),#17266);
#9430=REPRESENTATION('density',(#9271),#17266);
#9431=REPRESENTATION('material name',(#9532),#17267);
#9432=REPRESENTATION('density',(#9272),#17267);
#9433=REPRESENTATION('material name',(#9533),#17268);
#9434=REPRESENTATION('density',(#9273),#17268);
#9435=REPRESENTATION('material name',(#9534),#17269);
#9436=REPRESENTATION('density',(#9274),#17269);
#9437=REPRESENTATION('material name',(#9535),#17270);
#9438=REPRESENTATION('density',(#9275),#17270);
#9439=REPRESENTATION('material name',(#9536),#17271);
#9440=REPRESENTATION('density',(#9276),#17271);
#9441=REPRESENTATION('material name',(#9537),#17272);
#9442=REPRESENTATION('density',(#9277),#17272);
#9443=REPRESENTATION('material name',(#9538),#17273);
#9444=REPRESENTATION('density',(#9278),#17273);
#9445=REPRESENTATION('material name',(#9539),#17274);
#9446=REPRESENTATION('density',(#9279),#17274);
#9447=REPRESENTATION('material name',(#9540),#17275);
#9448=REPRESENTATION('density',(#9280),#17275);
#9449=REPRESENTATION('material name',(#9541),#17277);
#9450=REPRESENTATION('density',(#9281),#17277);
#9451=REPRESENTATION('material name',(#9542),#17278);
#9452=REPRESENTATION('density',(#9282),#17278);
#9453=REPRESENTATION('material name',(#9543),#17279);
#9454=REPRESENTATION('density',(#9283),#17279);
#9455=REPRESENTATION('material name',(#9544),#17280);
#9456=REPRESENTATION('density',(#9284),#17280);
#9457=REPRESENTATION('material name',(#9545),#17281);
#9458=REPRESENTATION('density',(#9285),#17281);
#9459=REPRESENTATION('material name',(#9546),#17282);
#9460=REPRESENTATION('density',(#9286),#17282);
#9461=REPRESENTATION('material name',(#9547),#17283);
#9462=REPRESENTATION('density',(#9287),#17283);
#9463=REPRESENTATION('material name',(#9548),#17284);
#9464=REPRESENTATION('density',(#9288),#17284);
#9465=REPRESENTATION('material name',(#9549),#17285);
#9466=REPRESENTATION('density',(#9289),#17285);
#9467=REPRESENTATION('material name',(#9550),#17287);
#9468=REPRESENTATION('density',(#9290),#17287);
#9469=REPRESENTATION('material name',(#9551),#17288);
#9470=REPRESENTATION('density',(#9291),#17288);
#9471=REPRESENTATION('material name',(#9552),#17289);
#9472=REPRESENTATION('density',(#9292),#17289);
#9473=REPRESENTATION('material name',(#9553),#17290);
#9474=REPRESENTATION('density',(#9293),#17290);
#9475=REPRESENTATION('material name',(#9554),#17291);
#9476=REPRESENTATION('density',(#9294),#17291);
#9477=REPRESENTATION('material name',(#9555),#17292);
#9478=REPRESENTATION('density',(#9295),#17292);
#9479=REPRESENTATION('material name',(#9556),#17293);
#9480=REPRESENTATION('density',(#9296),#17293);
#9481=REPRESENTATION('material name',(#9557),#17294);
#9482=REPRESENTATION('density',(#9297),#17294);
#9483=REPRESENTATION('material name',(#9558),#17295);
#9484=REPRESENTATION('density',(#9298),#17295);
#9485=REPRESENTATION('material name',(#9559),#17296);
#9486=REPRESENTATION('density',(#9299),#17296);
#9487=REPRESENTATION('material name',(#9560),#17297);
#9488=REPRESENTATION('density',(#9300),#17297);
#9489=REPRESENTATION('material name',(#9561),#17299);
#9490=REPRESENTATION('density',(#9301),#17299);
#9491=REPRESENTATION('material name',(#9562),#17300);
#9492=REPRESENTATION('density',(#9302),#17300);
#9493=REPRESENTATION('material name',(#9563),#17301);
#9494=REPRESENTATION('density',(#9303),#17301);
#9495=REPRESENTATION('material name',(#9564),#17302);
#9496=REPRESENTATION('density',(#9304),#17302);
#9497=REPRESENTATION('material name',(#9565),#17303);
#9498=REPRESENTATION('density',(#9305),#17303);
#9499=REPRESENTATION('material name',(#9566),#17305);
#9500=REPRESENTATION('density',(#9306),#17305);
#9501=REPRESENTATION('material name',(#9567),#17306);
#9502=REPRESENTATION('density',(#9307),#17306);
#9503=REPRESENTATION('material name',(#9568),#17307);
#9504=REPRESENTATION('density',(#9308),#17307);
#9505=REPRESENTATION('material name',(#9569),#17308);
#9506=REPRESENTATION('density',(#9309),#17308);
#9507=REPRESENTATION('material name',(#9570),#17309);
#9508=REPRESENTATION('density',(#9310),#17309);
#9509=REPRESENTATION('material name',(#9571),#17311);
#9510=REPRESENTATION('density',(#9311),#17311);
#9511=REPRESENTATION('material name',(#9572),#17312);
#9512=REPRESENTATION('density',(#9312),#17312);
#9513=REPRESENTATION('material name',(#9573),#17313);
#9514=REPRESENTATION('density',(#9313),#17313);
#9515=REPRESENTATION('material name',(#9574),#17314);
#9516=REPRESENTATION('density',(#9314),#17314);
#9517=REPRESENTATION('material name',(#9575),#17315);
#9518=REPRESENTATION('density',(#9315),#17315);
#9519=REPRESENTATION('material name',(#9576),#17316);
#9520=REPRESENTATION('density',(#9316),#17316);
#9521=REPRESENTATION('material name',(#9577),#17317);
#9522=REPRESENTATION('density',(#9317),#17317);
#9523=REPRESENTATION('material name',(#9578),#17319);
#9524=REPRESENTATION('density',(#9318),#17319);
#9525=REPRESENTATION('material name',(#9579),#17320);
#9526=REPRESENTATION('density',(#9319),#17320);
#9527=REPRESENTATION('material name',(#9580),#17321);
#9528=REPRESENTATION('density',(#9320),#17321);
#9529=DESCRIPTIVE_REPRESENTATION_ITEM('Steel','Steel');
#9530=DESCRIPTIVE_REPRESENTATION_ITEM('Steel','Steel');
#9531=DESCRIPTIVE_REPRESENTATION_ITEM('Steel','Steel');
#9532=DESCRIPTIVE_REPRESENTATION_ITEM('Steel','Steel');
#9533=DESCRIPTIVE_REPRESENTATION_ITEM('Steel','Steel');
#9534=DESCRIPTIVE_REPRESENTATION_ITEM('Steel','Steel');
#9535=DESCRIPTIVE_REPRESENTATION_ITEM('Steel','Steel');
#9536=DESCRIPTIVE_REPRESENTATION_ITEM('Steel','Steel');
#9537=DESCRIPTIVE_REPRESENTATION_ITEM('Steel','Steel');
#9538=DESCRIPTIVE_REPRESENTATION_ITEM('Steel','Steel');
#9539=DESCRIPTIVE_REPRESENTATION_ITEM('Steel','Steel');
#9540=DESCRIPTIVE_REPRESENTATION_ITEM('Steel','Steel');
#9541=DESCRIPTIVE_REPRESENTATION_ITEM('Steel','Steel');
#9542=DESCRIPTIVE_REPRESENTATION_ITEM('Steel','Steel');
#9543=DESCRIPTIVE_REPRESENTATION_ITEM('Steel','Steel');
#9544=DESCRIPTIVE_REPRESENTATION_ITEM('Steel','Steel');
#9545=DESCRIPTIVE_REPRESENTATION_ITEM('Steel','Steel');
#9546=DESCRIPTIVE_REPRESENTATION_ITEM('Steel','Steel');
#9547=DESCRIPTIVE_REPRESENTATION_ITEM('Steel','Steel');
#9548=DESCRIPTIVE_REPRESENTATION_ITEM('Steel','Steel');
#9549=DESCRIPTIVE_REPRESENTATION_ITEM('Steel','Steel');
#9550=DESCRIPTIVE_REPRESENTATION_ITEM('Steel','Steel');
#9551=DESCRIPTIVE_REPRESENTATION_ITEM('Steel','Steel');
#9552=DESCRIPTIVE_REPRESENTATION_ITEM('Steel','Steel');
#9553=DESCRIPTIVE_REPRESENTATION_ITEM('Steel','Steel');
#9554=DESCRIPTIVE_REPRESENTATION_ITEM('Steel','Steel');
#9555=DESCRIPTIVE_REPRESENTATION_ITEM('Steel','Steel');
#9556=DESCRIPTIVE_REPRESENTATION_ITEM('Steel','Steel');
#9557=DESCRIPTIVE_REPRESENTATION_ITEM('Steel','Steel');
#9558=DESCRIPTIVE_REPRESENTATION_ITEM('Steel','Steel');
#9559=DESCRIPTIVE_REPRESENTATION_ITEM('Steel','Steel');
#9560=DESCRIPTIVE_REPRESENTATION_ITEM('Steel','Steel');
#9561=DESCRIPTIVE_REPRESENTATION_ITEM('Steel','Steel');
#9562=DESCRIPTIVE_REPRESENTATION_ITEM('Steel','Steel');
#9563=DESCRIPTIVE_REPRESENTATION_ITEM('Steel','Steel');
#9564=DESCRIPTIVE_REPRESENTATION_ITEM('Steel','Steel');
#9565=DESCRIPTIVE_REPRESENTATION_ITEM('Steel','Steel');
#9566=DESCRIPTIVE_REPRESENTATION_ITEM('Steel','Steel');
#9567=DESCRIPTIVE_REPRESENTATION_ITEM('Steel','Steel');
#9568=DESCRIPTIVE_REPRESENTATION_ITEM('Steel','Steel');
#9569=DESCRIPTIVE_REPRESENTATION_ITEM('Steel','Steel');
#9570=DESCRIPTIVE_REPRESENTATION_ITEM('Steel','Steel');
#9571=DESCRIPTIVE_REPRESENTATION_ITEM('Steel','Steel');
#9572=DESCRIPTIVE_REPRESENTATION_ITEM('Steel','Steel');
#9573=DESCRIPTIVE_REPRESENTATION_ITEM('Steel','Steel');
#9574=DESCRIPTIVE_REPRESENTATION_ITEM('Steel','Steel');
#9575=DESCRIPTIVE_REPRESENTATION_ITEM('Steel','Steel');
#9576=DESCRIPTIVE_REPRESENTATION_ITEM('Steel','Steel');
#9577=DESCRIPTIVE_REPRESENTATION_ITEM('Steel','Steel');
#9578=DESCRIPTIVE_REPRESENTATION_ITEM('Steel','Steel');
#9579=DESCRIPTIVE_REPRESENTATION_ITEM('Steel','Steel');
#9580=DESCRIPTIVE_REPRESENTATION_ITEM('Steel','Steel');
#9581=PROPERTY_DEFINITION('material property','material name',#17621);
#9582=PROPERTY_DEFINITION('material property','density of part',#17621);
#9583=PROPERTY_DEFINITION('material property','material name',#17622);
#9584=PROPERTY_DEFINITION('material property','density of part',#17622);
#9585=PROPERTY_DEFINITION('material property','material name',#17623);
#9586=PROPERTY_DEFINITION('material property','density of part',#17623);
#9587=PROPERTY_DEFINITION('material property','material name',#17624);
#9588=PROPERTY_DEFINITION('material property','density of part',#17624);
#9589=PROPERTY_DEFINITION('material property','material name',#17625);
#9590=PROPERTY_DEFINITION('material property','density of part',#17625);
#9591=PROPERTY_DEFINITION('material property','material name',#17626);
#9592=PROPERTY_DEFINITION('material property','density of part',#17626);
#9593=PROPERTY_DEFINITION('material property','material name',#17627);
#9594=PROPERTY_DEFINITION('material property','density of part',#17627);
#9595=PROPERTY_DEFINITION('material property','material name',#17628);
#9596=PROPERTY_DEFINITION('material property','density of part',#17628);
#9597=PROPERTY_DEFINITION('material property','material name',#17629);
#9598=PROPERTY_DEFINITION('material property','density of part',#17629);
#9599=PROPERTY_DEFINITION('material property','material name',#17630);
#9600=PROPERTY_DEFINITION('material property','density of part',#17630);
#9601=PROPERTY_DEFINITION('material property','material name',#17631);
#9602=PROPERTY_DEFINITION('material property','density of part',#17631);
#9603=PROPERTY_DEFINITION('material property','material name',#17632);
#9604=PROPERTY_DEFINITION('material property','density of part',#17632);
#9605=PROPERTY_DEFINITION('material property','material name',#17634);
#9606=PROPERTY_DEFINITION('material property','density of part',#17634);
#9607=PROPERTY_DEFINITION('material property','material name',#17635);
#9608=PROPERTY_DEFINITION('material property','density of part',#17635);
#9609=PROPERTY_DEFINITION('material property','material name',#17636);
#9610=PROPERTY_DEFINITION('material property','density of part',#17636);
#9611=PROPERTY_DEFINITION('material property','material name',#17637);
#9612=PROPERTY_DEFINITION('material property','density of part',#17637);
#9613=PROPERTY_DEFINITION('material property','material name',#17638);
#9614=PROPERTY_DEFINITION('material property','density of part',#17638);
#9615=PROPERTY_DEFINITION('material property','material name',#17639);
#9616=PROPERTY_DEFINITION('material property','density of part',#17639);
#9617=PROPERTY_DEFINITION('material property','material name',#17640);
#9618=PROPERTY_DEFINITION('material property','density of part',#17640);
#9619=PROPERTY_DEFINITION('material property','material name',#17641);
#9620=PROPERTY_DEFINITION('material property','density of part',#17641);
#9621=PROPERTY_DEFINITION('material property','material name',#17642);
#9622=PROPERTY_DEFINITION('material property','density of part',#17642);
#9623=PROPERTY_DEFINITION('material property','material name',#17644);
#9624=PROPERTY_DEFINITION('material property','density of part',#17644);
#9625=PROPERTY_DEFINITION('material property','material name',#17645);
#9626=PROPERTY_DEFINITION('material property','density of part',#17645);
#9627=PROPERTY_DEFINITION('material property','material name',#17646);
#9628=PROPERTY_DEFINITION('material property','density of part',#17646);
#9629=PROPERTY_DEFINITION('material property','material name',#17647);
#9630=PROPERTY_DEFINITION('material property','density of part',#17647);
#9631=PROPERTY_DEFINITION('material property','material name',#17648);
#9632=PROPERTY_DEFINITION('material property','density of part',#17648);
#9633=PROPERTY_DEFINITION('material property','material name',#17649);
#9634=PROPERTY_DEFINITION('material property','density of part',#17649);
#9635=PROPERTY_DEFINITION('material property','material name',#17650);
#9636=PROPERTY_DEFINITION('material property','density of part',#17650);
#9637=PROPERTY_DEFINITION('material property','material name',#17651);
#9638=PROPERTY_DEFINITION('material property','density of part',#17651);
#9639=PROPERTY_DEFINITION('material property','material name',#17652);
#9640=PROPERTY_DEFINITION('material property','density of part',#17652);
#9641=PROPERTY_DEFINITION('material property','material name',#17653);
#9642=PROPERTY_DEFINITION('material property','density of part',#17653);
#9643=PROPERTY_DEFINITION('material property','material name',#17654);
#9644=PROPERTY_DEFINITION('material property','density of part',#17654);
#9645=PROPERTY_DEFINITION('material property','material name',#17656);
#9646=PROPERTY_DEFINITION('material property','density of part',#17656);
#9647=PROPERTY_DEFINITION('material property','material name',#17657);
#9648=PROPERTY_DEFINITION('material property','density of part',#17657);
#9649=PROPERTY_DEFINITION('material property','material name',#17658);
#9650=PROPERTY_DEFINITION('material property','density of part',#17658);
#9651=PROPERTY_DEFINITION('material property','material name',#17659);
#9652=PROPERTY_DEFINITION('material property','density of part',#17659);
#9653=PROPERTY_DEFINITION('material property','material name',#17660);
#9654=PROPERTY_DEFINITION('material property','density of part',#17660);
#9655=PROPERTY_DEFINITION('material property','material name',#17662);
#9656=PROPERTY_DEFINITION('material property','density of part',#17662);
#9657=PROPERTY_DEFINITION('material property','material name',#17663);
#9658=PROPERTY_DEFINITION('material property','density of part',#17663);
#9659=PROPERTY_DEFINITION('material property','material name',#17664);
#9660=PROPERTY_DEFINITION('material property','density of part',#17664);
#9661=PROPERTY_DEFINITION('material property','material name',#17665);
#9662=PROPERTY_DEFINITION('material property','density of part',#17665);
#9663=PROPERTY_DEFINITION('material property','material name',#17666);
#9664=PROPERTY_DEFINITION('material property','density of part',#17666);
#9665=PROPERTY_DEFINITION('material property','material name',#17668);
#9666=PROPERTY_DEFINITION('material property','density of part',#17668);
#9667=PROPERTY_DEFINITION('material property','material name',#17669);
#9668=PROPERTY_DEFINITION('material property','density of part',#17669);
#9669=PROPERTY_DEFINITION('material property','material name',#17670);
#9670=PROPERTY_DEFINITION('material property','density of part',#17670);
#9671=PROPERTY_DEFINITION('material property','material name',#17671);
#9672=PROPERTY_DEFINITION('material property','density of part',#17671);
#9673=PROPERTY_DEFINITION('material property','material name',#17672);
#9674=PROPERTY_DEFINITION('material property','density of part',#17672);
#9675=PROPERTY_DEFINITION('material property','material name',#17673);
#9676=PROPERTY_DEFINITION('material property','density of part',#17673);
#9677=PROPERTY_DEFINITION('material property','material name',#17674);
#9678=PROPERTY_DEFINITION('material property','density of part',#17674);
#9679=PROPERTY_DEFINITION('material property','material name',#17676);
#9680=PROPERTY_DEFINITION('material property','density of part',#17676);
#9681=PROPERTY_DEFINITION('material property','material name',#17677);
#9682=PROPERTY_DEFINITION('material property','density of part',#17677);
#9683=PROPERTY_DEFINITION('material property','material name',#17678);
#9684=PROPERTY_DEFINITION('material property','density of part',#17678);
#9685=AXIS2_PLACEMENT_3D('',#13731,#10830,#10831);
#9686=AXIS2_PLACEMENT_3D('',#13732,#10832,#10833);
#9687=AXIS2_PLACEMENT_3D('',#13733,#10834,#10835);
#9688=AXIS2_PLACEMENT_3D('',#13734,#10836,#10837);
#9689=AXIS2_PLACEMENT_3D('',#13736,#10838,#10839);
#9690=AXIS2_PLACEMENT_3D('',#13739,#10841,#10842);
#9691=AXIS2_PLACEMENT_3D('',#13740,#10843,#10844);
#9692=AXIS2_PLACEMENT_3D('',#13742,#10845,#10846);
#9693=AXIS2_PLACEMENT_3D('',#13745,#10848,#10849);
#9694=AXIS2_PLACEMENT_3D('',#13746,#10850,#10851);
#9695=AXIS2_PLACEMENT_3D('',#13748,#10852,#10853);
#9696=AXIS2_PLACEMENT_3D('',#13751,#10855,#10856);
#9697=AXIS2_PLACEMENT_3D('',#13752,#10857,#10858);
#9698=AXIS2_PLACEMENT_3D('',#13754,#10859,#10860);
#9699=AXIS2_PLACEMENT_3D('',#13757,#10862,#10863);
#9700=AXIS2_PLACEMENT_3D('',#13758,#10864,#10865);
#9701=AXIS2_PLACEMENT_3D('',#13760,#10866,#10867);
#9702=AXIS2_PLACEMENT_3D('',#13763,#10869,#10870);
#9703=AXIS2_PLACEMENT_3D('',#13764,#10871,#10872);
#9704=AXIS2_PLACEMENT_3D('',#13766,#10873,#10874);
#9705=AXIS2_PLACEMENT_3D('',#13769,#10876,#10877);
#9706=AXIS2_PLACEMENT_3D('',#13770,#10878,#10879);
#9707=AXIS2_PLACEMENT_3D('',#13772,#10880,#10881);
#9708=AXIS2_PLACEMENT_3D('',#13775,#10883,#10884);
#9709=AXIS2_PLACEMENT_3D('',#13776,#10885,#10886);
#9710=AXIS2_PLACEMENT_3D('',#13778,#10887,#10888);
#9711=AXIS2_PLACEMENT_3D('',#13781,#10890,#10891);
#9712=AXIS2_PLACEMENT_3D('',#13782,#10892,#10893);
#9713=AXIS2_PLACEMENT_3D('',#13784,#10894,#10895);
#9714=AXIS2_PLACEMENT_3D('',#13787,#10897,#10898);
#9715=AXIS2_PLACEMENT_3D('',#13788,#10899,#10900);
#9716=AXIS2_PLACEMENT_3D('',#13790,#10901,#10902);
#9717=AXIS2_PLACEMENT_3D('',#13793,#10904,#10905);
#9718=AXIS2_PLACEMENT_3D('',#13794,#10906,#10907);
#9719=AXIS2_PLACEMENT_3D('',#13796,#10908,#10909);
#9720=AXIS2_PLACEMENT_3D('',#13799,#10911,#10912);
#9721=AXIS2_PLACEMENT_3D('',#13800,#10913,#10914);
#9722=AXIS2_PLACEMENT_3D('',#13802,#10915,#10916);
#9723=AXIS2_PLACEMENT_3D('',#13805,#10918,#10919);
#9724=AXIS2_PLACEMENT_3D('',#13806,#10920,#10921);
#9725=AXIS2_PLACEMENT_3D('',#13815,#10926,#10927);
#9726=AXIS2_PLACEMENT_3D('',#13821,#10931,#10932);
#9727=AXIS2_PLACEMENT_3D('',#13827,#10936,#10937);
#9728=AXIS2_PLACEMENT_3D('',#13830,#10940,#10941);
#9729=AXIS2_PLACEMENT_3D('',#13831,#10942,#10943);
#9730=AXIS2_PLACEMENT_3D('',#13832,#10944,#10945);
#9731=AXIS2_PLACEMENT_3D('',#13833,#10946,#10947);
#9732=AXIS2_PLACEMENT_3D('',#13835,#10948,#10949);
#9733=AXIS2_PLACEMENT_3D('',#13838,#10951,#10952);
#9734=AXIS2_PLACEMENT_3D('',#13839,#10953,#10954);
#9735=AXIS2_PLACEMENT_3D('',#13840,#10955,#10956);
#9736=AXIS2_PLACEMENT_3D('',#13842,#10957,#10958);
#9737=AXIS2_PLACEMENT_3D('',#13845,#10960,#10961);
#9738=AXIS2_PLACEMENT_3D('',#13846,#10962,#10963);
#9739=AXIS2_PLACEMENT_3D('',#13847,#10964,#10965);
#9740=AXIS2_PLACEMENT_3D('',#13849,#10966,#10967);
#9741=AXIS2_PLACEMENT_3D('',#13852,#10969,#10970);
#9742=AXIS2_PLACEMENT_3D('',#13853,#10971,#10972);
#9743=AXIS2_PLACEMENT_3D('',#13855,#10973,#10974);
#9744=AXIS2_PLACEMENT_3D('',#13856,#10975,#10976);
#9745=AXIS2_PLACEMENT_3D('',#13858,#10977,#10978);
#9746=AXIS2_PLACEMENT_3D('',#13861,#10980,#10981);
#9747=AXIS2_PLACEMENT_3D('',#13862,#10982,#10983);
#9748=AXIS2_PLACEMENT_3D('',#13864,#10984,#10985);
#9749=AXIS2_PLACEMENT_3D('',#13865,#10986,#10987);
#9750=AXIS2_PLACEMENT_3D('',#13867,#10988,#10989);
#9751=AXIS2_PLACEMENT_3D('',#13870,#10991,#10992);
#9752=AXIS2_PLACEMENT_3D('',#13871,#10993,#10994);
#9753=AXIS2_PLACEMENT_3D('',#13873,#10995,#10996);
#9754=AXIS2_PLACEMENT_3D('',#13874,#10997,#10998);
#9755=AXIS2_PLACEMENT_3D('',#13876,#10999,#11000);
#9756=AXIS2_PLACEMENT_3D('',#13879,#11002,#11003);
#9757=AXIS2_PLACEMENT_3D('',#13880,#11004,#11005);
#9758=AXIS2_PLACEMENT_3D('',#13882,#11006,#11007);
#9759=AXIS2_PLACEMENT_3D('',#13883,#11008,#11009);
#9760=AXIS2_PLACEMENT_3D('',#13885,#11010,#11011);
#9761=AXIS2_PLACEMENT_3D('',#13887,#11013,#11014);
#9762=AXIS2_PLACEMENT_3D('',#13889,#11015,#11016);
#9763=AXIS2_PLACEMENT_3D('',#13891,#11018,#11019);
#9764=AXIS2_PLACEMENT_3D('',#13893,#11020,#11021);
#9765=AXIS2_PLACEMENT_3D('',#13895,#11023,#11024);
#9766=AXIS2_PLACEMENT_3D('',#13897,#11025,#11026);
#9767=AXIS2_PLACEMENT_3D('',#13899,#11028,#11029);
#9768=AXIS2_PLACEMENT_3D('',#13908,#11034,#11035);
#9769=AXIS2_PLACEMENT_3D('',#13914,#11039,#11040);
#9770=AXIS2_PLACEMENT_3D('',#13920,#11044,#11045);
#9771=AXIS2_PLACEMENT_3D('',#13923,#11048,#11049);
#9772=AXIS2_PLACEMENT_3D('',#13924,#11050,#11051);
#9773=AXIS2_PLACEMENT_3D('',#13925,#11052,#11053);
#9774=AXIS2_PLACEMENT_3D('',#13926,#11054,#11055);
#9775=AXIS2_PLACEMENT_3D('',#13928,#11056,#11057);
#9776=AXIS2_PLACEMENT_3D('',#13931,#11059,#11060);
#9777=AXIS2_PLACEMENT_3D('',#13932,#11061,#11062);
#9778=AXIS2_PLACEMENT_3D('',#13934,#11063,#11064);
#9779=AXIS2_PLACEMENT_3D('',#13937,#11066,#11067);
#9780=AXIS2_PLACEMENT_3D('',#13938,#11068,#11069);
#9781=AXIS2_PLACEMENT_3D('',#13939,#11070,#11071);
#9782=AXIS2_PLACEMENT_3D('',#13940,#11072,#11073);
#9783=AXIS2_PLACEMENT_3D('',#13941,#11074,#11075);
#9784=AXIS2_PLACEMENT_3D('',#13943,#11076,#11077);
#9785=AXIS2_PLACEMENT_3D('',#13946,#11079,#11080);
#9786=AXIS2_PLACEMENT_3D('',#13947,#11081,#11082);
#9787=AXIS2_PLACEMENT_3D('',#13949,#11083,#11084);
#9788=AXIS2_PLACEMENT_3D('',#13952,#11086,#11087);
#9789=AXIS2_PLACEMENT_3D('',#13953,#11088,#11089);
#9790=AXIS2_PLACEMENT_3D('',#13954,#11090,#11091);
#9791=AXIS2_PLACEMENT_3D('',#13955,#11092,#11093);
#9792=AXIS2_PLACEMENT_3D('',#13956,#11094,#11095);
#9793=AXIS2_PLACEMENT_3D('',#13958,#11096,#11097);
#9794=AXIS2_PLACEMENT_3D('',#13961,#11099,#11100);
#9795=AXIS2_PLACEMENT_3D('',#13962,#11101,#11102);
#9796=AXIS2_PLACEMENT_3D('',#13963,#11103,#11104);
#9797=AXIS2_PLACEMENT_3D('',#13965,#11105,#11106);
#9798=AXIS2_PLACEMENT_3D('',#13968,#11108,#11109);
#9799=AXIS2_PLACEMENT_3D('',#13969,#11110,#11111);
#9800=AXIS2_PLACEMENT_3D('',#13970,#11112,#11113);
#9801=AXIS2_PLACEMENT_3D('',#13972,#11114,#11115);
#9802=AXIS2_PLACEMENT_3D('',#13975,#11117,#11118);
#9803=AXIS2_PLACEMENT_3D('',#13976,#11119,#11120);
#9804=AXIS2_PLACEMENT_3D('',#13978,#11121,#11122);
#9805=AXIS2_PLACEMENT_3D('',#13979,#11123,#11124);
#9806=AXIS2_PLACEMENT_3D('',#13981,#11125,#11126);
#9807=AXIS2_PLACEMENT_3D('',#13984,#11128,#11129);
#9808=AXIS2_PLACEMENT_3D('',#13985,#11130,#11131);
#9809=AXIS2_PLACEMENT_3D('',#13987,#11132,#11133);
#9810=AXIS2_PLACEMENT_3D('',#13988,#11134,#11135);
#9811=AXIS2_PLACEMENT_3D('',#13990,#11136,#11137);
#9812=AXIS2_PLACEMENT_3D('',#13993,#11139,#11140);
#9813=AXIS2_PLACEMENT_3D('',#13994,#11141,#11142);
#9814=AXIS2_PLACEMENT_3D('',#13996,#11143,#11144);
#9815=AXIS2_PLACEMENT_3D('',#13997,#11145,#11146);
#9816=AXIS2_PLACEMENT_3D('',#13999,#11147,#11148);
#9817=AXIS2_PLACEMENT_3D('',#14002,#11150,#11151);
#9818=AXIS2_PLACEMENT_3D('',#14003,#11152,#11153);
#9819=AXIS2_PLACEMENT_3D('',#14005,#11154,#11155);
#9820=AXIS2_PLACEMENT_3D('',#14006,#11156,#11157);
#9821=AXIS2_PLACEMENT_3D('',#14008,#11158,#11159);
#9822=AXIS2_PLACEMENT_3D('',#14010,#11161,#11162);
#9823=AXIS2_PLACEMENT_3D('',#14012,#11163,#11164);
#9824=AXIS2_PLACEMENT_3D('',#14014,#11166,#11167);
#9825=AXIS2_PLACEMENT_3D('',#14016,#11168,#11169);
#9826=AXIS2_PLACEMENT_3D('',#14018,#11171,#11172);
#9827=AXIS2_PLACEMENT_3D('',#14020,#11173,#11174);
#9828=AXIS2_PLACEMENT_3D('',#14022,#11176,#11177);
#9829=AXIS2_PLACEMENT_3D('',#14031,#11182,#11183);
#9830=AXIS2_PLACEMENT_3D('',#14037,#11187,#11188);
#9831=AXIS2_PLACEMENT_3D('',#14043,#11192,#11193);
#9832=AXIS2_PLACEMENT_3D('',#14046,#11196,#11197);
#9833=AXIS2_PLACEMENT_3D('',#14047,#11198,#11199);
#9834=AXIS2_PLACEMENT_3D('',#14048,#11200,#11201);
#9835=AXIS2_PLACEMENT_3D('',#14049,#11202,#11203);
#9836=AXIS2_PLACEMENT_3D('',#14051,#11204,#11205);
#9837=AXIS2_PLACEMENT_3D('',#14054,#11207,#11208);
#9838=AXIS2_PLACEMENT_3D('',#14055,#11209,#11210);
#9839=AXIS2_PLACEMENT_3D('',#14057,#11211,#11212);
#9840=AXIS2_PLACEMENT_3D('',#14060,#11214,#11215);
#9841=AXIS2_PLACEMENT_3D('',#14061,#11216,#11217);
#9842=AXIS2_PLACEMENT_3D('',#14062,#11218,#11219);
#9843=AXIS2_PLACEMENT_3D('',#14063,#11220,#11221);
#9844=AXIS2_PLACEMENT_3D('',#14064,#11222,#11223);
#9845=AXIS2_PLACEMENT_3D('',#14066,#11224,#11225);
#9846=AXIS2_PLACEMENT_3D('',#14069,#11227,#11228);
#9847=AXIS2_PLACEMENT_3D('',#14070,#11229,#11230);
#9848=AXIS2_PLACEMENT_3D('',#14072,#11231,#11232);
#9849=AXIS2_PLACEMENT_3D('',#14075,#11234,#11235);
#9850=AXIS2_PLACEMENT_3D('',#14076,#11236,#11237);
#9851=AXIS2_PLACEMENT_3D('',#14077,#11238,#11239);
#9852=AXIS2_PLACEMENT_3D('',#14078,#11240,#11241);
#9853=AXIS2_PLACEMENT_3D('',#14079,#11242,#11243);
#9854=AXIS2_PLACEMENT_3D('',#14084,#11245,#11246);
#9855=AXIS2_PLACEMENT_3D('',#14087,#11248,#11249);
#9856=AXIS2_PLACEMENT_3D('',#14088,#11250,#11251);
#9857=AXIS2_PLACEMENT_3D('',#14090,#11252,#11253);
#9858=AXIS2_PLACEMENT_3D('',#14093,#11255,#11256);
#9859=AXIS2_PLACEMENT_3D('',#14095,#11258,#11259);
#9860=AXIS2_PLACEMENT_3D('',#14097,#11260,#11261);
#9861=AXIS2_PLACEMENT_3D('',#14098,#11262,#11263);
#9862=AXIS2_PLACEMENT_3D('',#14099,#11264,#11265);
#9863=AXIS2_PLACEMENT_3D('',#14101,#11267,#11268);
#9864=AXIS2_PLACEMENT_3D('',#14102,#11269,#11270);
#9865=AXIS2_PLACEMENT_3D('',#14104,#11271,#11272);
#9866=AXIS2_PLACEMENT_3D('',#14105,#11273,#11274);
#9867=AXIS2_PLACEMENT_3D('',#14117,#11281,#11282);
#9868=AXIS2_PLACEMENT_3D('',#14119,#11283,#11284);
#9869=AXIS2_PLACEMENT_3D('',#14121,#11285,#11286);
#9870=AXIS2_PLACEMENT_3D('',#14123,#11287,#11288);
#9871=AXIS2_PLACEMENT_3D('',#14124,#11289,#11290);
#9872=AXIS2_PLACEMENT_3D('',#14126,#11291,#11292);
#9873=AXIS2_PLACEMENT_3D('',#14128,#11294,#11295);
#9874=AXIS2_PLACEMENT_3D('',#14130,#11296,#11297);
#9875=AXIS2_PLACEMENT_3D('',#14132,#11299,#11300);
#9876=AXIS2_PLACEMENT_3D('',#14134,#11301,#11302);
#9877=AXIS2_PLACEMENT_3D('',#14136,#11304,#11305);
#9878=AXIS2_PLACEMENT_3D('',#14137,#11306,#11307);
#9879=AXIS2_PLACEMENT_3D('',#14139,#11308,#11309);
#9880=AXIS2_PLACEMENT_3D('',#14141,#11311,#11312);
#9881=AXIS2_PLACEMENT_3D('',#14142,#11313,#11314);
#9882=AXIS2_PLACEMENT_3D('',#14144,#11315,#11316);
#9883=AXIS2_PLACEMENT_3D('',#14146,#11318,#11319);
#9884=AXIS2_PLACEMENT_3D('',#14147,#11320,#11321);
#9885=AXIS2_PLACEMENT_3D('',#14149,#11322,#11323);
#9886=AXIS2_PLACEMENT_3D('',#14151,#11325,#11326);
#9887=AXIS2_PLACEMENT_3D('',#14152,#11327,#11328);
#9888=AXIS2_PLACEMENT_3D('',#14158,#11332,#11333);
#9889=AXIS2_PLACEMENT_3D('',#14162,#11336,#11337);
#9890=AXIS2_PLACEMENT_3D('',#14166,#11340,#11341);
#9891=AXIS2_PLACEMENT_3D('',#14168,#11343,#11344);
#9892=AXIS2_PLACEMENT_3D('',#14169,#11345,#11346);
#9893=AXIS2_PLACEMENT_3D('',#14170,#11347,#11348);
#9894=AXIS2_PLACEMENT_3D('',#14175,#11350,#11351);
#9895=AXIS2_PLACEMENT_3D('',#14178,#11353,#11354);
#9896=AXIS2_PLACEMENT_3D('',#14179,#11355,#11356);
#9897=AXIS2_PLACEMENT_3D('',#14181,#11357,#11358);
#9898=AXIS2_PLACEMENT_3D('',#14184,#11360,#11361);
#9899=AXIS2_PLACEMENT_3D('',#14186,#11363,#11364);
#9900=AXIS2_PLACEMENT_3D('',#14188,#11365,#11366);
#9901=AXIS2_PLACEMENT_3D('',#14189,#11367,#11368);
#9902=AXIS2_PLACEMENT_3D('',#14190,#11369,#11370);
#9903=AXIS2_PLACEMENT_3D('',#14192,#11372,#11373);
#9904=AXIS2_PLACEMENT_3D('',#14193,#11374,#11375);
#9905=AXIS2_PLACEMENT_3D('',#14195,#11376,#11377);
#9906=AXIS2_PLACEMENT_3D('',#14196,#11378,#11379);
#9907=AXIS2_PLACEMENT_3D('',#14208,#11386,#11387);
#9908=AXIS2_PLACEMENT_3D('',#14210,#11388,#11389);
#9909=AXIS2_PLACEMENT_3D('',#14212,#11390,#11391);
#9910=AXIS2_PLACEMENT_3D('',#14214,#11392,#11393);
#9911=AXIS2_PLACEMENT_3D('',#14215,#11394,#11395);
#9912=AXIS2_PLACEMENT_3D('',#14217,#11396,#11397);
#9913=AXIS2_PLACEMENT_3D('',#14219,#11399,#11400);
#9914=AXIS2_PLACEMENT_3D('',#14221,#11401,#11402);
#9915=AXIS2_PLACEMENT_3D('',#14223,#11404,#11405);
#9916=AXIS2_PLACEMENT_3D('',#14225,#11406,#11407);
#9917=AXIS2_PLACEMENT_3D('',#14227,#11409,#11410);
#9918=AXIS2_PLACEMENT_3D('',#14228,#11411,#11412);
#9919=AXIS2_PLACEMENT_3D('',#14230,#11413,#11414);
#9920=AXIS2_PLACEMENT_3D('',#14232,#11416,#11417);
#9921=AXIS2_PLACEMENT_3D('',#14233,#11418,#11419);
#9922=AXIS2_PLACEMENT_3D('',#14235,#11420,#11421);
#9923=AXIS2_PLACEMENT_3D('',#14237,#11423,#11424);
#9924=AXIS2_PLACEMENT_3D('',#14238,#11425,#11426);
#9925=AXIS2_PLACEMENT_3D('',#14240,#11427,#11428);
#9926=AXIS2_PLACEMENT_3D('',#14242,#11430,#11431);
#9927=AXIS2_PLACEMENT_3D('',#14243,#11432,#11433);
#9928=AXIS2_PLACEMENT_3D('',#14249,#11437,#11438);
#9929=AXIS2_PLACEMENT_3D('',#14253,#11441,#11442);
#9930=AXIS2_PLACEMENT_3D('',#14257,#11445,#11446);
#9931=AXIS2_PLACEMENT_3D('',#14259,#11448,#11449);
#9932=AXIS2_PLACEMENT_3D('',#14260,#11450,#11451);
#9933=AXIS2_PLACEMENT_3D('',#14261,#11452,#11453);
#9934=AXIS2_PLACEMENT_3D('',#14270,#11458,#11459);
#9935=AXIS2_PLACEMENT_3D('',#14276,#11463,#11464);
#9936=AXIS2_PLACEMENT_3D('',#14282,#11468,#11469);
#9937=AXIS2_PLACEMENT_3D('',#14285,#11472,#11473);
#9938=AXIS2_PLACEMENT_3D('',#14286,#11474,#11475);
#9939=AXIS2_PLACEMENT_3D('',#14287,#11476,#11477);
#9940=AXIS2_PLACEMENT_3D('',#14288,#11478,#11479);
#9941=AXIS2_PLACEMENT_3D('',#14297,#11484,#11485);
#9942=AXIS2_PLACEMENT_3D('',#14303,#11489,#11490);
#9943=AXIS2_PLACEMENT_3D('',#14309,#11494,#11495);
#9944=AXIS2_PLACEMENT_3D('',#14312,#11498,#11499);
#9945=AXIS2_PLACEMENT_3D('',#14313,#11500,#11501);
#9946=AXIS2_PLACEMENT_3D('',#14314,#11502,#11503);
#9947=AXIS2_PLACEMENT_3D('',#14315,#11504,#11505);
#9948=AXIS2_PLACEMENT_3D('',#14317,#11506,#11507);
#9949=AXIS2_PLACEMENT_3D('',#14318,#11508,#11509);
#9950=AXIS2_PLACEMENT_3D('',#14320,#11510,#11511);
#9951=AXIS2_PLACEMENT_3D('',#14322,#11513,#11514);
#9952=AXIS2_PLACEMENT_3D('',#14324,#11515,#11516);
#9953=AXIS2_PLACEMENT_3D('',#14326,#11518,#11519);
#9954=AXIS2_PLACEMENT_3D('',#14328,#11520,#11521);
#9955=AXIS2_PLACEMENT_3D('',#14330,#11523,#11524);
#9956=AXIS2_PLACEMENT_3D('',#14332,#11525,#11526);
#9957=AXIS2_PLACEMENT_3D('',#14333,#11527,#11528);
#9958=AXIS2_PLACEMENT_3D('',#14335,#11529,#11530);
#9959=AXIS2_PLACEMENT_3D('',#14337,#11532,#11533);
#9960=AXIS2_PLACEMENT_3D('',#14339,#11534,#11535);
#9961=AXIS2_PLACEMENT_3D('',#14341,#11537,#11538);
#9962=AXIS2_PLACEMENT_3D('',#14343,#11539,#11540);
#9963=AXIS2_PLACEMENT_3D('',#14345,#11542,#11543);
#9964=AXIS2_PLACEMENT_3D('',#14346,#11544,#11545);
#9965=AXIS2_PLACEMENT_3D('',#14355,#11550,#11551);
#9966=AXIS2_PLACEMENT_3D('',#14361,#11555,#11556);
#9967=AXIS2_PLACEMENT_3D('',#14367,#11560,#11561);
#9968=AXIS2_PLACEMENT_3D('',#14373,#11565,#11566);
#9969=AXIS2_PLACEMENT_3D('',#14379,#11570,#11571);
#9970=AXIS2_PLACEMENT_3D('',#14382,#11574,#11575);
#9971=AXIS2_PLACEMENT_3D('',#14383,#11576,#11577);
#9972=AXIS2_PLACEMENT_3D('',#14384,#11578,#11579);
#9973=AXIS2_PLACEMENT_3D('',#14385,#11580,#11581);
#9974=AXIS2_PLACEMENT_3D('',#14386,#11582,#11583);
#9975=AXIS2_PLACEMENT_3D('',#14388,#11584,#11585);
#9976=AXIS2_PLACEMENT_3D('',#14391,#11587,#11588);
#9977=AXIS2_PLACEMENT_3D('',#14392,#11589,#11590);
#9978=AXIS2_PLACEMENT_3D('',#14394,#11591,#11592);
#9979=AXIS2_PLACEMENT_3D('',#14397,#11594,#11595);
#9980=AXIS2_PLACEMENT_3D('',#14398,#11596,#11597);
#9981=AXIS2_PLACEMENT_3D('',#14401,#11598,#11599);
#9982=AXIS2_PLACEMENT_3D('',#14402,#11600,#11601);
#9983=AXIS2_PLACEMENT_3D('',#14408,#11604,#11605);
#9984=AXIS2_PLACEMENT_3D('',#14409,#11606,#11607);
#9985=AXIS2_PLACEMENT_3D('',#14414,#11609,#11610);
#9986=AXIS2_PLACEMENT_3D('',#14416,#11612,#11613);
#9987=AXIS2_PLACEMENT_3D('',#14421,#11615,#11616);
#9988=AXIS2_PLACEMENT_3D('',#14423,#11618,#11619);
#9989=AXIS2_PLACEMENT_3D('',#14426,#11622,#11623);
#9990=AXIS2_PLACEMENT_3D('',#14432,#11626,#11627);
#9991=AXIS2_PLACEMENT_3D('',#14433,#11628,#11629);
#9992=AXIS2_PLACEMENT_3D('',#14436,#11632,#11633);
#9993=AXIS2_PLACEMENT_3D('',#14446,#11638,#11639);
#9994=AXIS2_PLACEMENT_3D('',#14448,#11640,#11641);
#9995=AXIS2_PLACEMENT_3D('',#14459,#11648,#11649);
#9996=AXIS2_PLACEMENT_3D('',#14460,#11650,#11651);
#9997=AXIS2_PLACEMENT_3D('',#14461,#11652,#11653);
#9998=AXIS2_PLACEMENT_3D('',#14462,#11654,#11655);
#9999=AXIS2_PLACEMENT_3D('',#14463,#11656,#11657);
#10000=AXIS2_PLACEMENT_3D('',#14464,#11658,#11659);
#10001=AXIS2_PLACEMENT_3D('',#14473,#11664,#11665);
#10002=AXIS2_PLACEMENT_3D('',#14479,#11669,#11670);
#10003=AXIS2_PLACEMENT_3D('',#14485,#11674,#11675);
#10004=AXIS2_PLACEMENT_3D('',#14488,#11678,#11679);
#10005=AXIS2_PLACEMENT_3D('',#14489,#11680,#11681);
#10006=AXIS2_PLACEMENT_3D('',#14491,#11682,#11683);
#10007=AXIS2_PLACEMENT_3D('',#14493,#11685,#11686);
#10008=AXIS2_PLACEMENT_3D('',#14495,#11687,#11688);
#10009=AXIS2_PLACEMENT_3D('',#14497,#11690,#11691);
#10010=AXIS2_PLACEMENT_3D('',#14503,#11695,#11696);
#10011=AXIS2_PLACEMENT_3D('',#14507,#11699,#11700);
#10012=AXIS2_PLACEMENT_3D('',#14511,#11703,#11704);
#10013=AXIS2_PLACEMENT_3D('',#14513,#11706,#11707);
#10014=AXIS2_PLACEMENT_3D('',#14514,#11708,#11709);
#10015=AXIS2_PLACEMENT_3D('',#14515,#11710,#11711);
#10016=AXIS2_PLACEMENT_3D('',#14517,#11712,#11713);
#10017=AXIS2_PLACEMENT_3D('',#14520,#11715,#11716);
#10018=AXIS2_PLACEMENT_3D('',#14521,#11717,#11718);
#10019=AXIS2_PLACEMENT_3D('',#14523,#11719,#11720);
#10020=AXIS2_PLACEMENT_3D('',#14524,#11721,#11722);
#10021=AXIS2_PLACEMENT_3D('',#14527,#11723,#11724);
#10022=AXIS2_PLACEMENT_3D('',#14529,#11725,#11726);
#10023=AXIS2_PLACEMENT_3D('',#14530,#11727,#11728);
#10024=AXIS2_PLACEMENT_3D('',#14531,#11729,#11730);
#10025=AXIS2_PLACEMENT_3D('',#14609,#11732,#11733);
#10026=AXIS2_PLACEMENT_3D('',#14687,#11735,#11736);
#10027=AXIS2_PLACEMENT_3D('',#14689,#11737,#11738);
#10028=AXIS2_PLACEMENT_3D('',#14692,#11740,#11741);
#10029=AXIS2_PLACEMENT_3D('',#14857,#11742,#11743);
#10030=AXIS2_PLACEMENT_3D('',#14894,#11745,#11746);
#10031=AXIS2_PLACEMENT_3D('',#14931,#11748,#11749);
#10032=AXIS2_PLACEMENT_3D('',#14968,#11751,#11752);
#10033=AXIS2_PLACEMENT_3D('',#15005,#11754,#11755);
#10034=AXIS2_PLACEMENT_3D('',#15007,#11756,#11757);
#10035=AXIS2_PLACEMENT_3D('',#15008,#11758,#11759);
#10036=AXIS2_PLACEMENT_3D('',#15010,#11760,#11761);
#10037=AXIS2_PLACEMENT_3D('',#15011,#11762,#11763);
#10038=AXIS2_PLACEMENT_3D('',#15013,#11764,#11765);
#10039=AXIS2_PLACEMENT_3D('',#15015,#11767,#11768);
#10040=AXIS2_PLACEMENT_3D('',#15017,#11769,#11770);
#10041=AXIS2_PLACEMENT_3D('',#15018,#11771,#11772);
#10042=AXIS2_PLACEMENT_3D('',#15020,#11774,#11775);
#10043=AXIS2_PLACEMENT_3D('',#15021,#11776,#11777);
#10044=AXIS2_PLACEMENT_3D('',#15022,#11778,#11779);
#10045=AXIS2_PLACEMENT_3D('',#15023,#11780,#11781);
#10046=AXIS2_PLACEMENT_3D('',#15025,#11782,#11783);
#10047=AXIS2_PLACEMENT_3D('',#15028,#11785,#11786);
#10048=AXIS2_PLACEMENT_3D('',#15029,#11787,#11788);
#10049=AXIS2_PLACEMENT_3D('',#15031,#11789,#11790);
#10050=AXIS2_PLACEMENT_3D('',#15034,#11792,#11793);
#10051=AXIS2_PLACEMENT_3D('',#15035,#11794,#11795);
#10052=AXIS2_PLACEMENT_3D('',#15036,#11796,#11797);
#10053=AXIS2_PLACEMENT_3D('',#15037,#11798,#11799);
#10054=AXIS2_PLACEMENT_3D('',#15038,#11800,#11801);
#10055=AXIS2_PLACEMENT_3D('',#15047,#11806,#11807);
#10056=AXIS2_PLACEMENT_3D('',#15053,#11811,#11812);
#10057=AXIS2_PLACEMENT_3D('',#15059,#11816,#11817);
#10058=AXIS2_PLACEMENT_3D('',#15065,#11821,#11822);
#10059=AXIS2_PLACEMENT_3D('',#15071,#11826,#11827);
#10060=AXIS2_PLACEMENT_3D('',#15074,#11830,#11831);
#10061=AXIS2_PLACEMENT_3D('',#15075,#11832,#11833);
#10062=AXIS2_PLACEMENT_3D('',#15076,#11834,#11835);
#10063=AXIS2_PLACEMENT_3D('',#15078,#11836,#11837);
#10064=AXIS2_PLACEMENT_3D('',#15079,#11838,#11839);
#10065=AXIS2_PLACEMENT_3D('',#15081,#11840,#11841);
#10066=AXIS2_PLACEMENT_3D('',#15082,#11842,#11843);
#10067=AXIS2_PLACEMENT_3D('',#15084,#11844,#11845);
#10068=AXIS2_PLACEMENT_3D('',#15086,#11847,#11848);
#10069=AXIS2_PLACEMENT_3D('',#15088,#11849,#11850);
#10070=AXIS2_PLACEMENT_3D('',#15090,#11852,#11853);
#10071=AXIS2_PLACEMENT_3D('',#15092,#11854,#11855);
#10072=AXIS2_PLACEMENT_3D('',#15094,#11857,#11858);
#10073=AXIS2_PLACEMENT_3D('',#15096,#11859,#11860);
#10074=AXIS2_PLACEMENT_3D('',#15097,#11861,#11862);
#10075=AXIS2_PLACEMENT_3D('',#15099,#11863,#11864);
#10076=AXIS2_PLACEMENT_3D('',#15101,#11866,#11867);
#10077=AXIS2_PLACEMENT_3D('',#15103,#11869,#11870);
#10078=AXIS2_PLACEMENT_3D('',#15104,#11871,#11872);
#10079=AXIS2_PLACEMENT_3D('',#15108,#11874,#11875);
#10080=AXIS2_PLACEMENT_3D('',#15109,#11876,#11877);
#10081=AXIS2_PLACEMENT_3D('',#15113,#11879,#11880);
#10082=AXIS2_PLACEMENT_3D('',#15115,#11882,#11883);
#10083=AXIS2_PLACEMENT_3D('',#15120,#11885,#11886);
#10084=AXIS2_PLACEMENT_3D('',#15123,#11888,#11889);
#10085=AXIS2_PLACEMENT_3D('',#15124,#11890,#11891);
#10086=AXIS2_PLACEMENT_3D('',#15126,#11893,#11894);
#10087=AXIS2_PLACEMENT_3D('',#15137,#11900,#11901);
#10088=AXIS2_PLACEMENT_3D('',#15138,#11902,#11903);
#10089=AXIS2_PLACEMENT_3D('',#15145,#11907,#11908);
#10090=AXIS2_PLACEMENT_3D('',#15146,#11909,#11910);
#10091=AXIS2_PLACEMENT_3D('',#15157,#11916,#11917);
#10092=AXIS2_PLACEMENT_3D('',#15158,#11918,#11919);
#10093=AXIS2_PLACEMENT_3D('',#15160,#11920,#11921);
#10094=AXIS2_PLACEMENT_3D('',#15163,#11923,#11924);
#10095=AXIS2_PLACEMENT_3D('',#15164,#11925,#11926);
#10096=AXIS2_PLACEMENT_3D('',#15167,#11928,#11929);
#10097=AXIS2_PLACEMENT_3D('',#15168,#11930,#11931);
#10098=AXIS2_PLACEMENT_3D('',#15170,#11932,#11933);
#10099=AXIS2_PLACEMENT_3D('',#15172,#11935,#11936);
#10100=AXIS2_PLACEMENT_3D('',#15174,#11937,#11938);
#10101=AXIS2_PLACEMENT_3D('',#15176,#11940,#11941);
#10102=AXIS2_PLACEMENT_3D('',#15178,#11942,#11943);
#10103=AXIS2_PLACEMENT_3D('',#15181,#11945,#11946);
#10104=AXIS2_PLACEMENT_3D('',#15182,#11947,#11948);
#10105=AXIS2_PLACEMENT_3D('',#15199,#11958,#11959);
#10106=AXIS2_PLACEMENT_3D('',#15203,#11962,#11963);
#10107=AXIS2_PLACEMENT_3D('',#15207,#11966,#11967);
#10108=AXIS2_PLACEMENT_3D('',#15209,#11969,#11970);
#10109=AXIS2_PLACEMENT_3D('',#15213,#11973,#11974);
#10110=AXIS2_PLACEMENT_3D('',#15217,#11977,#11978);
#10111=AXIS2_PLACEMENT_3D('',#15221,#11981,#11982);
#10112=AXIS2_PLACEMENT_3D('',#15225,#11985,#11986);
#10113=AXIS2_PLACEMENT_3D('',#15229,#11989,#11990);
#10114=AXIS2_PLACEMENT_3D('',#15231,#11992,#11993);
#10115=AXIS2_PLACEMENT_3D('',#15232,#11994,#11995);
#10116=AXIS2_PLACEMENT_3D('',#15233,#11996,#11997);
#10117=AXIS2_PLACEMENT_3D('',#15235,#11998,#11999);
#10118=AXIS2_PLACEMENT_3D('',#15238,#12001,#12002);
#10119=AXIS2_PLACEMENT_3D('',#15239,#12003,#12004);
#10120=AXIS2_PLACEMENT_3D('',#15242,#12006,#12007);
#10121=AXIS2_PLACEMENT_3D('',#15243,#12008,#12009);
#10122=AXIS2_PLACEMENT_3D('',#15245,#12010,#12011);
#10123=AXIS2_PLACEMENT_3D('',#15246,#12012,#12013);
#10124=AXIS2_PLACEMENT_3D('',#15249,#12015,#12016);
#10125=AXIS2_PLACEMENT_3D('',#15250,#12017,#12018);
#10126=AXIS2_PLACEMENT_3D('',#15251,#12019,#12020);
#10127=AXIS2_PLACEMENT_3D('',#15252,#12021,#12022);
#10128=AXIS2_PLACEMENT_3D('',#15261,#12027,#12028);
#10129=AXIS2_PLACEMENT_3D('',#15267,#12032,#12033);
#10130=AXIS2_PLACEMENT_3D('',#15273,#12037,#12038);
#10131=AXIS2_PLACEMENT_3D('',#15279,#12042,#12043);
#10132=AXIS2_PLACEMENT_3D('',#15285,#12047,#12048);
#10133=AXIS2_PLACEMENT_3D('',#15288,#12051,#12052);
#10134=AXIS2_PLACEMENT_3D('',#15289,#12053,#12054);
#10135=AXIS2_PLACEMENT_3D('',#15290,#12055,#12056);
#10136=AXIS2_PLACEMENT_3D('',#15292,#12057,#12058);
#10137=AXIS2_PLACEMENT_3D('',#15293,#12059,#12060);
#10138=AXIS2_PLACEMENT_3D('',#15295,#12061,#12062);
#10139=AXIS2_PLACEMENT_3D('',#15296,#12063,#12064);
#10140=AXIS2_PLACEMENT_3D('',#15298,#12065,#12066);
#10141=AXIS2_PLACEMENT_3D('',#15300,#12068,#12069);
#10142=AXIS2_PLACEMENT_3D('',#15302,#12070,#12071);
#10143=AXIS2_PLACEMENT_3D('',#15304,#12073,#12074);
#10144=AXIS2_PLACEMENT_3D('',#15306,#12075,#12076);
#10145=AXIS2_PLACEMENT_3D('',#15308,#12078,#12079);
#10146=AXIS2_PLACEMENT_3D('',#15310,#12080,#12081);
#10147=AXIS2_PLACEMENT_3D('',#15311,#12082,#12083);
#10148=AXIS2_PLACEMENT_3D('',#15313,#12084,#12085);
#10149=AXIS2_PLACEMENT_3D('',#15315,#12087,#12088);
#10150=AXIS2_PLACEMENT_3D('',#15317,#12090,#12091);
#10151=AXIS2_PLACEMENT_3D('',#15318,#12092,#12093);
#10152=AXIS2_PLACEMENT_3D('',#15320,#12094,#12095);
#10153=AXIS2_PLACEMENT_3D('',#15321,#12096,#12097);
#10154=AXIS2_PLACEMENT_3D('',#15323,#12098,#12099);
#10155=AXIS2_PLACEMENT_3D('',#15325,#12101,#12102);
#10156=AXIS2_PLACEMENT_3D('',#15327,#12103,#12104);
#10157=AXIS2_PLACEMENT_3D('',#15329,#12106,#12107);
#10158=AXIS2_PLACEMENT_3D('',#15331,#12108,#12109);
#10159=AXIS2_PLACEMENT_3D('',#15333,#12111,#12112);
#10160=AXIS2_PLACEMENT_3D('',#15335,#12113,#12114);
#10161=AXIS2_PLACEMENT_3D('',#15336,#12115,#12116);
#10162=AXIS2_PLACEMENT_3D('',#15338,#12117,#12118);
#10163=AXIS2_PLACEMENT_3D('',#15340,#12120,#12121);
#10164=AXIS2_PLACEMENT_3D('',#15342,#12122,#12123);
#10165=AXIS2_PLACEMENT_3D('',#15344,#12125,#12126);
#10166=AXIS2_PLACEMENT_3D('',#15346,#12127,#12128);
#10167=AXIS2_PLACEMENT_3D('',#15348,#12130,#12131);
#10168=AXIS2_PLACEMENT_3D('',#15349,#12132,#12133);
#10169=AXIS2_PLACEMENT_3D('',#15358,#12138,#12139);
#10170=AXIS2_PLACEMENT_3D('',#15364,#12143,#12144);
#10171=AXIS2_PLACEMENT_3D('',#15370,#12148,#12149);
#10172=AXIS2_PLACEMENT_3D('',#15376,#12153,#12154);
#10173=AXIS2_PLACEMENT_3D('',#15382,#12158,#12159);
#10174=AXIS2_PLACEMENT_3D('',#15385,#12162,#12163);
#10175=AXIS2_PLACEMENT_3D('',#15386,#12164,#12165);
#10176=AXIS2_PLACEMENT_3D('',#15387,#12166,#12167);
#10177=AXIS2_PLACEMENT_3D('',#15388,#12168,#12169);
#10178=AXIS2_PLACEMENT_3D('',#15390,#12170,#12171);
#10179=AXIS2_PLACEMENT_3D('',#15391,#12172,#12173);
#10180=AXIS2_PLACEMENT_3D('',#15393,#12174,#12175);
#10181=AXIS2_PLACEMENT_3D('',#15396,#12177,#12178);
#10182=AXIS2_PLACEMENT_3D('',#15397,#12179,#12180);
#10183=AXIS2_PLACEMENT_3D('',#15399,#12182,#12183);
#10184=AXIS2_PLACEMENT_3D('',#15400,#12184,#12185);
#10185=AXIS2_PLACEMENT_3D('',#15401,#12186,#12187);
#10186=AXIS2_PLACEMENT_3D('',#15402,#12188,#12189);
#10187=AXIS2_PLACEMENT_3D('',#15411,#12194,#12195);
#10188=AXIS2_PLACEMENT_3D('',#15413,#12196,#12197);
#10189=AXIS2_PLACEMENT_3D('',#15417,#12200,#12201);
#10190=AXIS2_PLACEMENT_3D('',#15423,#12205,#12206);
#10191=AXIS2_PLACEMENT_3D('',#15425,#12208,#12209);
#10192=AXIS2_PLACEMENT_3D('',#15427,#12210,#12211);
#10193=AXIS2_PLACEMENT_3D('',#15430,#12213,#12214);
#10194=AXIS2_PLACEMENT_3D('',#15431,#12215,#12216);
#10195=AXIS2_PLACEMENT_3D('',#15432,#12217,#12218);
#10196=AXIS2_PLACEMENT_3D('',#15433,#12219,#12220);
#10197=AXIS2_PLACEMENT_3D('',#15434,#12221,#12222);
#10198=AXIS2_PLACEMENT_3D('',#15435,#12223,#12224);
#10199=AXIS2_PLACEMENT_3D('',#15439,#12226,#12227);
#10200=AXIS2_PLACEMENT_3D('',#15440,#12228,#12229);
#10201=AXIS2_PLACEMENT_3D('',#15457,#12230,#12231);
#10202=AXIS2_PLACEMENT_3D('',#15498,#12233,#12234);
#10203=AXIS2_PLACEMENT_3D('',#15513,#12235,#12236);
#10204=AXIS2_PLACEMENT_3D('',#15515,#12238,#12239);
#10205=AXIS2_PLACEMENT_3D('',#15517,#12240,#12241);
#10206=AXIS2_PLACEMENT_3D('',#15520,#12243,#12244);
#10207=AXIS2_PLACEMENT_3D('',#15521,#12245,#12246);
#10208=AXIS2_PLACEMENT_3D('',#15523,#12247,#12248);
#10209=AXIS2_PLACEMENT_3D('',#15526,#12250,#12251);
#10210=AXIS2_PLACEMENT_3D('',#15527,#12252,#12253);
#10211=AXIS2_PLACEMENT_3D('',#15528,#12254,#12255);
#10212=AXIS2_PLACEMENT_3D('',#15529,#12256,#12257);
#10213=AXIS2_PLACEMENT_3D('',#15530,#12258,#12259);
#10214=AXIS2_PLACEMENT_3D('',#15534,#12261,#12262);
#10215=AXIS2_PLACEMENT_3D('',#15535,#12263,#12264);
#10216=AXIS2_PLACEMENT_3D('',#15552,#12265,#12266);
#10217=AXIS2_PLACEMENT_3D('',#15593,#12268,#12269);
#10218=AXIS2_PLACEMENT_3D('',#15608,#12270,#12271);
#10219=AXIS2_PLACEMENT_3D('',#15610,#12273,#12274);
#10220=AXIS2_PLACEMENT_3D('',#15612,#12275,#12276);
#10221=AXIS2_PLACEMENT_3D('',#15615,#12278,#12279);
#10222=AXIS2_PLACEMENT_3D('',#15616,#12280,#12281);
#10223=AXIS2_PLACEMENT_3D('',#15618,#12282,#12283);
#10224=AXIS2_PLACEMENT_3D('',#15621,#12285,#12286);
#10225=AXIS2_PLACEMENT_3D('',#15622,#12287,#12288);
#10226=AXIS2_PLACEMENT_3D('',#15623,#12289,#12290);
#10227=AXIS2_PLACEMENT_3D('',#15624,#12291,#12292);
#10228=AXIS2_PLACEMENT_3D('',#15625,#12293,#12294);
#10229=AXIS2_PLACEMENT_3D('',#15627,#12295,#12296);
#10230=AXIS2_PLACEMENT_3D('',#15630,#12298,#12299);
#10231=AXIS2_PLACEMENT_3D('',#15631,#12300,#12301);
#10232=AXIS2_PLACEMENT_3D('',#15633,#12302,#12303);
#10233=AXIS2_PLACEMENT_3D('',#15636,#12305,#12306);
#10234=AXIS2_PLACEMENT_3D('',#15637,#12307,#12308);
#10235=AXIS2_PLACEMENT_3D('',#15638,#12309,#12310);
#10236=AXIS2_PLACEMENT_3D('',#15639,#12311,#12312);
#10237=AXIS2_PLACEMENT_3D('',#15640,#12313,#12314);
#10238=AXIS2_PLACEMENT_3D('',#15645,#12316,#12317);
#10239=AXIS2_PLACEMENT_3D('',#15648,#12319,#12320);
#10240=AXIS2_PLACEMENT_3D('',#15649,#12321,#12322);
#10241=AXIS2_PLACEMENT_3D('',#15650,#12323,#12324);
#10242=AXIS2_PLACEMENT_3D('',#15658,#12328,#12329);
#10243=AXIS2_PLACEMENT_3D('',#15659,#12330,#12331);
#10244=AXIS2_PLACEMENT_3D('',#15661,#12332,#12333);
#10245=AXIS2_PLACEMENT_3D('',#15664,#12335,#12336);
#10246=AXIS2_PLACEMENT_3D('',#15665,#12337,#12338);
#10247=AXIS2_PLACEMENT_3D('',#15666,#12339,#12340);
#10248=AXIS2_PLACEMENT_3D('',#15670,#12342,#12343);
#10249=AXIS2_PLACEMENT_3D('',#15671,#12344,#12345);
#10250=AXIS2_PLACEMENT_3D('',#15684,#12346,#12347);
#10251=AXIS2_PLACEMENT_3D('',#15738,#12350,#12351);
#10252=AXIS2_PLACEMENT_3D('',#15740,#12353,#12354);
#10253=AXIS2_PLACEMENT_3D('',#15742,#12355,#12356);
#10254=AXIS2_PLACEMENT_3D('',#15746,#12359,#12360);
#10255=AXIS2_PLACEMENT_3D('',#15747,#12361,#12362);
#10256=AXIS2_PLACEMENT_3D('',#15751,#12365,#12366);
#10257=AXIS2_PLACEMENT_3D('',#15755,#12369,#12370);
#10258=AXIS2_PLACEMENT_3D('',#15757,#12372,#12373);
#10259=AXIS2_PLACEMENT_3D('',#15759,#12374,#12375);
#10260=AXIS2_PLACEMENT_3D('',#15760,#12376,#12377);
#10261=AXIS2_PLACEMENT_3D('',#15761,#12378,#12379);
#10262=AXIS2_PLACEMENT_3D('',#15763,#12380,#12381);
#10263=AXIS2_PLACEMENT_3D('',#15765,#12382,#12383);
#10264=AXIS2_PLACEMENT_3D('',#15766,#12384,#12385);
#10265=AXIS2_PLACEMENT_3D('',#15768,#12387,#12388);
#10266=AXIS2_PLACEMENT_3D('',#15771,#12390,#12391);
#10267=AXIS2_PLACEMENT_3D('',#15772,#12392,#12393);
#10268=AXIS2_PLACEMENT_3D('',#15773,#12394,#12395);
#10269=AXIS2_PLACEMENT_3D('',#15774,#12396,#12397);
#10270=AXIS2_PLACEMENT_3D('',#15775,#12398,#12399);
#10271=AXIS2_PLACEMENT_3D('',#15776,#12400,#12401);
#10272=AXIS2_PLACEMENT_3D('',#15778,#12402,#12403);
#10273=AXIS2_PLACEMENT_3D('',#15781,#12405,#12406);
#10274=AXIS2_PLACEMENT_3D('',#15782,#12407,#12408);
#10275=AXIS2_PLACEMENT_3D('',#15783,#12409,#12410);
#10276=AXIS2_PLACEMENT_3D('',#15785,#12411,#12412);
#10277=AXIS2_PLACEMENT_3D('',#15787,#12413,#12414);
#10278=AXIS2_PLACEMENT_3D('',#15788,#12415,#12416);
#10279=AXIS2_PLACEMENT_3D('',#15790,#12417,#12418);
#10280=AXIS2_PLACEMENT_3D('',#15792,#12420,#12421);
#10281=AXIS2_PLACEMENT_3D('',#15793,#12422,#12423);
#10282=AXIS2_PLACEMENT_3D('',#15796,#12425,#12426);
#10283=AXIS2_PLACEMENT_3D('',#15797,#12427,#12428);
#10284=AXIS2_PLACEMENT_3D('',#15798,#12429,#12430);
#10285=AXIS2_PLACEMENT_3D('',#15799,#12431,#12432);
#10286=AXIS2_PLACEMENT_3D('',#15801,#12433,#12434);
#10287=AXIS2_PLACEMENT_3D('',#15804,#12436,#12437);
#10288=AXIS2_PLACEMENT_3D('',#15805,#12438,#12439);
#10289=AXIS2_PLACEMENT_3D('',#15807,#12440,#12441);
#10290=AXIS2_PLACEMENT_3D('',#15810,#12443,#12444);
#10291=AXIS2_PLACEMENT_3D('',#15811,#12445,#12446);
#10292=AXIS2_PLACEMENT_3D('',#15812,#12447,#12448);
#10293=AXIS2_PLACEMENT_3D('',#15813,#12449,#12450);
#10294=AXIS2_PLACEMENT_3D('',#15814,#12451,#12452);
#10295=AXIS2_PLACEMENT_3D('',#15816,#12453,#12454);
#10296=AXIS2_PLACEMENT_3D('',#15819,#12456,#12457);
#10297=AXIS2_PLACEMENT_3D('',#15820,#12458,#12459);
#10298=AXIS2_PLACEMENT_3D('',#15822,#12460,#12461);
#10299=AXIS2_PLACEMENT_3D('',#15825,#12463,#12464);
#10300=AXIS2_PLACEMENT_3D('',#15826,#12465,#12466);
#10301=AXIS2_PLACEMENT_3D('',#15827,#12467,#12468);
#10302=AXIS2_PLACEMENT_3D('',#15828,#12469,#12470);
#10303=AXIS2_PLACEMENT_3D('',#15829,#12471,#12472);
#10304=AXIS2_PLACEMENT_3D('',#15831,#12473,#12474);
#10305=AXIS2_PLACEMENT_3D('',#15834,#12476,#12477);
#10306=AXIS2_PLACEMENT_3D('',#15835,#12478,#12479);
#10307=AXIS2_PLACEMENT_3D('',#15837,#12480,#12481);
#10308=AXIS2_PLACEMENT_3D('',#15840,#12483,#12484);
#10309=AXIS2_PLACEMENT_3D('',#15841,#12485,#12486);
#10310=AXIS2_PLACEMENT_3D('',#15842,#12487,#12488);
#10311=AXIS2_PLACEMENT_3D('',#15843,#12489,#12490);
#10312=AXIS2_PLACEMENT_3D('',#15844,#12491,#12492);
#10313=AXIS2_PLACEMENT_3D('',#15861,#12501,#12502);
#10314=AXIS2_PLACEMENT_3D('',#15867,#12506,#12507);
#10315=AXIS2_PLACEMENT_3D('',#15871,#12510,#12511);
#10316=AXIS2_PLACEMENT_3D('',#15875,#12514,#12515);
#10317=AXIS2_PLACEMENT_3D('',#15879,#12518,#12519);
#10318=AXIS2_PLACEMENT_3D('',#15887,#12524,#12525);
#10319=AXIS2_PLACEMENT_3D('',#15889,#12527,#12528);
#10320=AXIS2_PLACEMENT_3D('',#15891,#12530,#12531);
#10321=AXIS2_PLACEMENT_3D('',#15893,#12533,#12534);
#10322=AXIS2_PLACEMENT_3D('',#15894,#12535,#12536);
#10323=AXIS2_PLACEMENT_3D('',#15895,#12537,#12538);
#10324=AXIS2_PLACEMENT_3D('',#15904,#12543,#12544);
#10325=AXIS2_PLACEMENT_3D('',#15910,#12548,#12549);
#10326=AXIS2_PLACEMENT_3D('',#15916,#12553,#12554);
#10327=AXIS2_PLACEMENT_3D('',#15922,#12558,#12559);
#10328=AXIS2_PLACEMENT_3D('',#15928,#12563,#12564);
#10329=AXIS2_PLACEMENT_3D('',#15931,#12567,#12568);
#10330=AXIS2_PLACEMENT_3D('',#15932,#12569,#12570);
#10331=AXIS2_PLACEMENT_3D('',#15934,#12571,#12572);
#10332=AXIS2_PLACEMENT_3D('',#15935,#12573,#12574);
#10333=AXIS2_PLACEMENT_3D('',#15937,#12575,#12576);
#10334=AXIS2_PLACEMENT_3D('',#15939,#12578,#12579);
#10335=AXIS2_PLACEMENT_3D('',#15941,#12580,#12581);
#10336=AXIS2_PLACEMENT_3D('',#15943,#12583,#12584);
#10337=AXIS2_PLACEMENT_3D('',#15945,#12585,#12586);
#10338=AXIS2_PLACEMENT_3D('',#15947,#12588,#12589);
#10339=AXIS2_PLACEMENT_3D('',#15948,#12590,#12591);
#10340=AXIS2_PLACEMENT_3D('',#15949,#12592,#12593);
#10341=AXIS2_PLACEMENT_3D('',#15950,#12594,#12595);
#10342=AXIS2_PLACEMENT_3D('',#15952,#12596,#12597);
#10343=AXIS2_PLACEMENT_3D('',#15955,#12599,#12600);
#10344=AXIS2_PLACEMENT_3D('',#15956,#12601,#12602);
#10345=AXIS2_PLACEMENT_3D('',#15958,#12603,#12604);
#10346=AXIS2_PLACEMENT_3D('',#15961,#12606,#12607);
#10347=AXIS2_PLACEMENT_3D('',#15962,#12608,#12609);
#10348=AXIS2_PLACEMENT_3D('',#15967,#12611,#12612);
#10349=AXIS2_PLACEMENT_3D('',#15970,#12614,#12615);
#10350=AXIS2_PLACEMENT_3D('',#15971,#12616,#12617);
#10351=AXIS2_PLACEMENT_3D('',#15975,#12619,#12620);
#10352=AXIS2_PLACEMENT_3D('',#15977,#12622,#12623);
#10353=AXIS2_PLACEMENT_3D('',#15981,#12626,#12627);
#10354=AXIS2_PLACEMENT_3D('',#15984,#12629,#12630);
#10355=AXIS2_PLACEMENT_3D('',#15985,#12631,#12632);
#10356=AXIS2_PLACEMENT_3D('',#15987,#12634,#12635);
#10357=AXIS2_PLACEMENT_3D('',#15988,#12636,#12637);
#10358=AXIS2_PLACEMENT_3D('',#15989,#12638,#12639);
#10359=AXIS2_PLACEMENT_3D('',#15991,#12640,#12641);
#10360=AXIS2_PLACEMENT_3D('',#15994,#12643,#12644);
#10361=AXIS2_PLACEMENT_3D('',#15995,#12645,#12646);
#10362=AXIS2_PLACEMENT_3D('',#15997,#12647,#12648);
#10363=AXIS2_PLACEMENT_3D('',#16000,#12650,#12651);
#10364=AXIS2_PLACEMENT_3D('',#16001,#12652,#12653);
#10365=AXIS2_PLACEMENT_3D('',#16002,#12654,#12655);
#10366=AXIS2_PLACEMENT_3D('',#16003,#12656,#12657);
#10367=AXIS2_PLACEMENT_3D('',#16004,#12658,#12659);
#10368=AXIS2_PLACEMENT_3D('',#16006,#12660,#12661);
#10369=AXIS2_PLACEMENT_3D('',#16009,#12663,#12664);
#10370=AXIS2_PLACEMENT_3D('',#16010,#12665,#12666);
#10371=AXIS2_PLACEMENT_3D('',#16012,#12667,#12668);
#10372=AXIS2_PLACEMENT_3D('',#16015,#12670,#12671);
#10373=AXIS2_PLACEMENT_3D('',#16016,#12672,#12673);
#10374=AXIS2_PLACEMENT_3D('',#16017,#12674,#12675);
#10375=AXIS2_PLACEMENT_3D('',#16018,#12676,#12677);
#10376=AXIS2_PLACEMENT_3D('',#16019,#12678,#12679);
#10377=AXIS2_PLACEMENT_3D('',#16021,#12680,#12681);
#10378=AXIS2_PLACEMENT_3D('',#16024,#12683,#12684);
#10379=AXIS2_PLACEMENT_3D('',#16025,#12685,#12686);
#10380=AXIS2_PLACEMENT_3D('',#16027,#12687,#12688);
#10381=AXIS2_PLACEMENT_3D('',#16030,#12690,#12691);
#10382=AXIS2_PLACEMENT_3D('',#16031,#12692,#12693);
#10383=AXIS2_PLACEMENT_3D('',#16032,#12694,#12695);
#10384=AXIS2_PLACEMENT_3D('',#16033,#12696,#12697);
#10385=AXIS2_PLACEMENT_3D('',#16034,#12698,#12699);
#10386=AXIS2_PLACEMENT_3D('',#16036,#12700,#12701);
#10387=AXIS2_PLACEMENT_3D('',#16039,#12703,#12704);
#10388=AXIS2_PLACEMENT_3D('',#16040,#12705,#12706);
#10389=AXIS2_PLACEMENT_3D('',#16042,#12707,#12708);
#10390=AXIS2_PLACEMENT_3D('',#16045,#12710,#12711);
#10391=AXIS2_PLACEMENT_3D('',#16046,#12712,#12713);
#10392=AXIS2_PLACEMENT_3D('',#16047,#12714,#12715);
#10393=AXIS2_PLACEMENT_3D('',#16048,#12716,#12717);
#10394=AXIS2_PLACEMENT_3D('',#16049,#12718,#12719);
#10395=AXIS2_PLACEMENT_3D('',#16050,#12720,#12721);
#10396=AXIS2_PLACEMENT_3D('',#16053,#12722,#12723);
#10397=AXIS2_PLACEMENT_3D('',#16054,#12724,#12725);
#10398=AXIS2_PLACEMENT_3D('',#16056,#12726,#12727);
#10399=AXIS2_PLACEMENT_3D('',#16058,#12728,#12729);
#10400=AXIS2_PLACEMENT_3D('',#16059,#12730,#12731);
#10401=AXIS2_PLACEMENT_3D('',#16060,#12732,#12733);
#10402=AXIS2_PLACEMENT_3D('',#16063,#12735,#12736);
#10403=AXIS2_PLACEMENT_3D('',#16064,#12737,#12738);
#10404=AXIS2_PLACEMENT_3D('',#16066,#12739,#12740);
#10405=AXIS2_PLACEMENT_3D('',#16069,#12742,#12743);
#10406=AXIS2_PLACEMENT_3D('',#16070,#12744,#12745);
#10407=AXIS2_PLACEMENT_3D('',#16073,#12747,#12748);
#10408=AXIS2_PLACEMENT_3D('',#16074,#12749,#12750);
#10409=AXIS2_PLACEMENT_3D('',#16075,#12751,#12752);
#10410=AXIS2_PLACEMENT_3D('',#16077,#12753,#12754);
#10411=AXIS2_PLACEMENT_3D('',#16079,#12756,#12757);
#10412=AXIS2_PLACEMENT_3D('',#16081,#12758,#12759);
#10413=AXIS2_PLACEMENT_3D('',#16082,#12760,#12761);
#10414=AXIS2_PLACEMENT_3D('',#16084,#12763,#12764);
#10415=AXIS2_PLACEMENT_3D('',#16085,#12765,#12766);
#10416=AXIS2_PLACEMENT_3D('',#16088,#12767,#12768);
#10417=AXIS2_PLACEMENT_3D('',#16089,#12769,#12770);
#10418=AXIS2_PLACEMENT_3D('',#16091,#12771,#12772);
#10419=AXIS2_PLACEMENT_3D('',#16093,#12773,#12774);
#10420=AXIS2_PLACEMENT_3D('',#16094,#12775,#12776);
#10421=AXIS2_PLACEMENT_3D('',#16095,#12777,#12778);
#10422=AXIS2_PLACEMENT_3D('',#16097,#12779,#12780);
#10423=AXIS2_PLACEMENT_3D('',#16099,#12782,#12783);
#10424=AXIS2_PLACEMENT_3D('',#16101,#12784,#12785);
#10425=AXIS2_PLACEMENT_3D('',#16103,#12786,#12787);
#10426=AXIS2_PLACEMENT_3D('',#16104,#12788,#12789);
#10427=AXIS2_PLACEMENT_3D('',#16106,#12790,#12791);
#10428=AXIS2_PLACEMENT_3D('',#16108,#12793,#12794);
#10429=AXIS2_PLACEMENT_3D('',#16110,#12795,#12796);
#10430=AXIS2_PLACEMENT_3D('',#16112,#12798,#12799);
#10431=AXIS2_PLACEMENT_3D('',#16114,#12800,#12801);
#10432=AXIS2_PLACEMENT_3D('',#16116,#12803,#12804);
#10433=AXIS2_PLACEMENT_3D('',#16117,#12805,#12806);
#10434=AXIS2_PLACEMENT_3D('',#16119,#12808,#12809);
#10435=AXIS2_PLACEMENT_3D('',#16120,#12810,#12811);
#10436=AXIS2_PLACEMENT_3D('',#16123,#12812,#12813);
#10437=AXIS2_PLACEMENT_3D('',#16124,#12814,#12815);
#10438=AXIS2_PLACEMENT_3D('',#16127,#12816,#12817);
#10439=AXIS2_PLACEMENT_3D('',#16128,#12818,#12819);
#10440=AXIS2_PLACEMENT_3D('',#16131,#12820,#12821);
#10441=AXIS2_PLACEMENT_3D('',#16132,#12822,#12823);
#10442=AXIS2_PLACEMENT_3D('',#16135,#12824,#12825);
#10443=AXIS2_PLACEMENT_3D('',#16136,#12826,#12827);
#10444=AXIS2_PLACEMENT_3D('',#16139,#12828,#12829);
#10445=AXIS2_PLACEMENT_3D('',#16140,#12830,#12831);
#10446=AXIS2_PLACEMENT_3D('',#16143,#12832,#12833);
#10447=AXIS2_PLACEMENT_3D('',#16144,#12834,#12835);
#10448=AXIS2_PLACEMENT_3D('',#16147,#12836,#12837);
#10449=AXIS2_PLACEMENT_3D('',#16148,#12838,#12839);
#10450=AXIS2_PLACEMENT_3D('',#16151,#12840,#12841);
#10451=AXIS2_PLACEMENT_3D('',#16152,#12842,#12843);
#10452=AXIS2_PLACEMENT_3D('',#16153,#12844,#12845);
#10453=AXIS2_PLACEMENT_3D('',#16179,#12846,#12847);
#10454=AXIS2_PLACEMENT_3D('',#16203,#12848,#12849);
#10455=AXIS2_PLACEMENT_3D('',#16204,#12850,#12851);
#10456=AXIS2_PLACEMENT_3D('',#16206,#12852,#12853);
#10457=AXIS2_PLACEMENT_3D('',#16231,#12854,#12855);
#10458=AXIS2_PLACEMENT_3D('',#16256,#12856,#12857);
#10459=AXIS2_PLACEMENT_3D('',#16272,#12859,#12860);
#10460=AXIS2_PLACEMENT_3D('',#16287,#12861,#12862);
#10461=AXIS2_PLACEMENT_3D('',#16312,#12863,#12864);
#10462=AXIS2_PLACEMENT_3D('',#16337,#12865,#12866);
#10463=AXIS2_PLACEMENT_3D('',#16362,#12867,#12868);
#10464=AXIS2_PLACEMENT_3D('',#16386,#12869,#12870);
#10465=AXIS2_PLACEMENT_3D('',#16387,#12871,#12872);
#10466=AXIS2_PLACEMENT_3D('',#16389,#12873,#12874);
#10467=AXIS2_PLACEMENT_3D('',#16390,#12875,#12876);
#10468=AXIS2_PLACEMENT_3D('',#16391,#12877,#12878);
#10469=AXIS2_PLACEMENT_3D('',#16415,#12879,#12880);
#10470=AXIS2_PLACEMENT_3D('',#16416,#12881,#12882);
#10471=AXIS2_PLACEMENT_3D('',#16418,#12883,#12884);
#10472=AXIS2_PLACEMENT_3D('',#16419,#12885,#12886);
#10473=AXIS2_PLACEMENT_3D('',#16420,#12887,#12888);
#10474=AXIS2_PLACEMENT_3D('',#16444,#12889,#12890);
#10475=AXIS2_PLACEMENT_3D('',#16445,#12891,#12892);
#10476=AXIS2_PLACEMENT_3D('',#16447,#12893,#12894);
#10477=AXIS2_PLACEMENT_3D('',#16448,#12895,#12896);
#10478=AXIS2_PLACEMENT_3D('',#16449,#12897,#12898);
#10479=AXIS2_PLACEMENT_3D('',#16464,#12899,#12900);
#10480=AXIS2_PLACEMENT_3D('',#16477,#12901,#12902);
#10481=AXIS2_PLACEMENT_3D('',#16479,#12903,#12904);
#10482=AXIS2_PLACEMENT_3D('',#16480,#12905,#12906);
#10483=AXIS2_PLACEMENT_3D('',#16481,#12907,#12908);
#10484=AXIS2_PLACEMENT_3D('',#16505,#12909,#12910);
#10485=AXIS2_PLACEMENT_3D('',#16506,#12911,#12912);
#10486=AXIS2_PLACEMENT_3D('',#16508,#12913,#12914);
#10487=AXIS2_PLACEMENT_3D('',#16509,#12915,#12916);
#10488=AXIS2_PLACEMENT_3D('',#16510,#12917,#12918);
#10489=AXIS2_PLACEMENT_3D('',#16534,#12919,#12920);
#10490=AXIS2_PLACEMENT_3D('',#16535,#12921,#12922);
#10491=AXIS2_PLACEMENT_3D('',#16537,#12923,#12924);
#10492=AXIS2_PLACEMENT_3D('',#16538,#12925,#12926);
#10493=AXIS2_PLACEMENT_3D('',#16539,#12927,#12928);
#10494=AXIS2_PLACEMENT_3D('',#16563,#12929,#12930);
#10495=AXIS2_PLACEMENT_3D('',#16564,#12931,#12932);
#10496=AXIS2_PLACEMENT_3D('',#16566,#12933,#12934);
#10497=AXIS2_PLACEMENT_3D('',#16569,#12936,#12937);
#10498=AXIS2_PLACEMENT_3D('',#16593,#12938,#12939);
#10499=AXIS2_PLACEMENT_3D('',#16594,#12940,#12941);
#10500=AXIS2_PLACEMENT_3D('',#16595,#12942,#12943);
#10501=AXIS2_PLACEMENT_3D('',#16596,#12944,#12945);
#10502=AXIS2_PLACEMENT_3D('',#16597,#12946,#12947);
#10503=AXIS2_PLACEMENT_3D('',#16598,#12948,#12949);
#10504=AXIS2_PLACEMENT_3D('',#16599,#12950,#12951);
#10505=AXIS2_PLACEMENT_3D('',#16600,#12952,#12953);
#10506=AXIS2_PLACEMENT_3D('',#16601,#12954,#12955);
#10507=AXIS2_PLACEMENT_3D('',#16603,#12956,#12957);
#10508=AXIS2_PLACEMENT_3D('',#16605,#12958,#12959);
#10509=AXIS2_PLACEMENT_3D('',#16606,#12960,#12961);
#10510=AXIS2_PLACEMENT_3D('',#16608,#12962,#12963);
#10511=AXIS2_PLACEMENT_3D('',#16610,#12965,#12966);
#10512=AXIS2_PLACEMENT_3D('',#16612,#12967,#12968);
#10513=AXIS2_PLACEMENT_3D('',#16613,#12969,#12970);
#10514=AXIS2_PLACEMENT_3D('',#16615,#12972,#12973);
#10515=AXIS2_PLACEMENT_3D('',#16617,#12974,#12975);
#10516=AXIS2_PLACEMENT_3D('',#16619,#12976,#12977);
#10517=AXIS2_PLACEMENT_3D('',#16620,#12978,#12979);
#10518=AXIS2_PLACEMENT_3D('',#16622,#12980,#12981);
#10519=AXIS2_PLACEMENT_3D('',#16624,#12983,#12984);
#10520=AXIS2_PLACEMENT_3D('',#16626,#12985,#12986);
#10521=AXIS2_PLACEMENT_3D('',#16627,#12987,#12988);
#10522=AXIS2_PLACEMENT_3D('',#16629,#12990,#12991);
#10523=AXIS2_PLACEMENT_3D('',#16630,#12992,#12993);
#10524=AXIS2_PLACEMENT_3D('',#16631,#12994,#12995);
#10525=AXIS2_PLACEMENT_3D('',#16632,#12996,#12997);
#10526=AXIS2_PLACEMENT_3D('',#16633,#12998,#12999);
#10527=AXIS2_PLACEMENT_3D('',#16634,#13000,#13001);
#10528=AXIS2_PLACEMENT_3D('',#16635,#13002,#13003);
#10529=AXIS2_PLACEMENT_3D('',#16636,#13004,#13005);
#10530=AXIS2_PLACEMENT_3D('',#16637,#13006,#13007);
#10531=AXIS2_PLACEMENT_3D('',#16638,#13008,#13009);
#10532=AXIS2_PLACEMENT_3D('',#16639,#13010,#13011);
#10533=AXIS2_PLACEMENT_3D('',#16640,#13012,#13013);
#10534=AXIS2_PLACEMENT_3D('',#16641,#13014,#13015);
#10535=AXIS2_PLACEMENT_3D('',#16642,#13016,#13017);
#10536=AXIS2_PLACEMENT_3D('',#16643,#13018,#13019);
#10537=AXIS2_PLACEMENT_3D('',#16645,#13020,#13021);
#10538=AXIS2_PLACEMENT_3D('',#16648,#13023,#13024);
#10539=AXIS2_PLACEMENT_3D('',#16649,#13025,#13026);
#10540=AXIS2_PLACEMENT_3D('',#16658,#13031,#13032);
#10541=AXIS2_PLACEMENT_3D('',#16664,#13036,#13037);
#10542=AXIS2_PLACEMENT_3D('',#16670,#13041,#13042);
#10543=AXIS2_PLACEMENT_3D('',#16672,#13044,#13045);
#10544=AXIS2_PLACEMENT_3D('',#16674,#13047,#13048);
#10545=AXIS2_PLACEMENT_3D('',#16676,#13049,#13050);
#10546=AXIS2_PLACEMENT_3D('',#16679,#13052,#13053);
#10547=AXIS2_PLACEMENT_3D('',#16680,#13054,#13055);
#10548=AXIS2_PLACEMENT_3D('',#16682,#13056,#13057);
#10549=AXIS2_PLACEMENT_3D('',#16685,#13059,#13060);
#10550=AXIS2_PLACEMENT_3D('',#16686,#13061,#13062);
#10551=AXIS2_PLACEMENT_3D('',#16688,#13063,#13064);
#10552=AXIS2_PLACEMENT_3D('',#16691,#13066,#13067);
#10553=AXIS2_PLACEMENT_3D('',#16692,#13068,#13069);
#10554=AXIS2_PLACEMENT_3D('',#16694,#13070,#13071);
#10555=AXIS2_PLACEMENT_3D('',#16697,#13073,#13074);
#10556=AXIS2_PLACEMENT_3D('',#16698,#13075,#13076);
#10557=AXIS2_PLACEMENT_3D('',#16700,#13077,#13078);
#10558=AXIS2_PLACEMENT_3D('',#16703,#13080,#13081);
#10559=AXIS2_PLACEMENT_3D('',#16704,#13082,#13083);
#10560=AXIS2_PLACEMENT_3D('',#16706,#13084,#13085);
#10561=AXIS2_PLACEMENT_3D('',#16709,#13087,#13088);
#10562=AXIS2_PLACEMENT_3D('',#16710,#13089,#13090);
#10563=AXIS2_PLACEMENT_3D('',#16719,#13095,#13096);
#10564=AXIS2_PLACEMENT_3D('',#16725,#13100,#13101);
#10565=AXIS2_PLACEMENT_3D('',#16731,#13105,#13106);
#10566=AXIS2_PLACEMENT_3D('',#16734,#13109,#13110);
#10567=AXIS2_PLACEMENT_3D('',#16735,#13111,#13112);
#10568=AXIS2_PLACEMENT_3D('',#16736,#13113,#13114);
#10569=AXIS2_PLACEMENT_3D('',#16737,#13115,#13116);
#10570=AXIS2_PLACEMENT_3D('',#16739,#13117,#13118);
#10571=AXIS2_PLACEMENT_3D('',#16742,#13120,#13121);
#10572=AXIS2_PLACEMENT_3D('',#16743,#13122,#13123);
#10573=AXIS2_PLACEMENT_3D('',#16745,#13124,#13125);
#10574=AXIS2_PLACEMENT_3D('',#16748,#13127,#13128);
#10575=AXIS2_PLACEMENT_3D('',#16749,#13129,#13130);
#10576=AXIS2_PLACEMENT_3D('',#16751,#13131,#13132);
#10577=AXIS2_PLACEMENT_3D('',#16754,#13134,#13135);
#10578=AXIS2_PLACEMENT_3D('',#16755,#13136,#13137);
#10579=AXIS2_PLACEMENT_3D('',#16757,#13138,#13139);
#10580=AXIS2_PLACEMENT_3D('',#16760,#13141,#13142);
#10581=AXIS2_PLACEMENT_3D('',#16761,#13143,#13144);
#10582=AXIS2_PLACEMENT_3D('',#16763,#13145,#13146);
#10583=AXIS2_PLACEMENT_3D('',#16766,#13148,#13149);
#10584=AXIS2_PLACEMENT_3D('',#16767,#13150,#13151);
#10585=AXIS2_PLACEMENT_3D('',#16769,#13152,#13153);
#10586=AXIS2_PLACEMENT_3D('',#16772,#13155,#13156);
#10587=AXIS2_PLACEMENT_3D('',#16773,#13157,#13158);
#10588=AXIS2_PLACEMENT_3D('',#16782,#13163,#13164);
#10589=AXIS2_PLACEMENT_3D('',#16788,#13168,#13169);
#10590=AXIS2_PLACEMENT_3D('',#16794,#13173,#13174);
#10591=AXIS2_PLACEMENT_3D('',#16797,#13177,#13178);
#10592=AXIS2_PLACEMENT_3D('',#16798,#13179,#13180);
#10593=AXIS2_PLACEMENT_3D('',#16799,#13181,#13182);
#10594=AXIS2_PLACEMENT_3D('',#16800,#13183,#13184);
#10595=AXIS2_PLACEMENT_3D('',#16802,#13185,#13186);
#10596=AXIS2_PLACEMENT_3D('',#16805,#13188,#13189);
#10597=AXIS2_PLACEMENT_3D('',#16806,#13190,#13191);
#10598=AXIS2_PLACEMENT_3D('',#16808,#13192,#13193);
#10599=AXIS2_PLACEMENT_3D('',#16811,#13195,#13196);
#10600=AXIS2_PLACEMENT_3D('',#16812,#13197,#13198);
#10601=AXIS2_PLACEMENT_3D('',#16814,#13199,#13200);
#10602=AXIS2_PLACEMENT_3D('',#16817,#13202,#13203);
#10603=AXIS2_PLACEMENT_3D('',#16818,#13204,#13205);
#10604=AXIS2_PLACEMENT_3D('',#16820,#13206,#13207);
#10605=AXIS2_PLACEMENT_3D('',#16823,#13209,#13210);
#10606=AXIS2_PLACEMENT_3D('',#16824,#13211,#13212);
#10607=AXIS2_PLACEMENT_3D('',#16826,#13213,#13214);
#10608=AXIS2_PLACEMENT_3D('',#16829,#13216,#13217);
#10609=AXIS2_PLACEMENT_3D('',#16830,#13218,#13219);
#10610=AXIS2_PLACEMENT_3D('',#16832,#13220,#13221);
#10611=AXIS2_PLACEMENT_3D('',#16835,#13223,#13224);
#10612=AXIS2_PLACEMENT_3D('',#16836,#13225,#13226);
#10613=AXIS2_PLACEMENT_3D('',#16845,#13231,#13232);
#10614=AXIS2_PLACEMENT_3D('',#16851,#13236,#13237);
#10615=AXIS2_PLACEMENT_3D('',#16857,#13241,#13242);
#10616=AXIS2_PLACEMENT_3D('',#16860,#13245,#13246);
#10617=AXIS2_PLACEMENT_3D('',#16861,#13247,#13248);
#10618=AXIS2_PLACEMENT_3D('',#16862,#13249,#13250);
#10619=AXIS2_PLACEMENT_3D('',#16863,#13251,#13252);
#10620=AXIS2_PLACEMENT_3D('',#16865,#13253,#13254);
#10621=AXIS2_PLACEMENT_3D('',#16868,#13256,#13257);
#10622=AXIS2_PLACEMENT_3D('',#16869,#13258,#13259);
#10623=AXIS2_PLACEMENT_3D('',#16870,#13260,#13261);
#10624=AXIS2_PLACEMENT_3D('',#16872,#13262,#13263);
#10625=AXIS2_PLACEMENT_3D('',#16874,#13264,#13265);
#10626=AXIS2_PLACEMENT_3D('',#16875,#13266,#13267);
#10627=AXIS2_PLACEMENT_3D('',#16878,#13269,#13270);
#10628=AXIS2_PLACEMENT_3D('',#16879,#13271,#13272);
#10629=AXIS2_PLACEMENT_3D('',#16880,#13273,#13274);
#10630=AXIS2_PLACEMENT_3D('',#16882,#13275,#13276);
#10631=AXIS2_PLACEMENT_3D('',#16884,#13278,#13279);
#10632=AXIS2_PLACEMENT_3D('',#16885,#13280,#13281);
#10633=AXIS2_PLACEMENT_3D('',#16886,#13282,#13283);
#10634=AXIS2_PLACEMENT_3D('',#16888,#13284,#13285);
#10635=AXIS2_PLACEMENT_3D('',#16891,#13287,#13288);
#10636=AXIS2_PLACEMENT_3D('',#16892,#13289,#13290);
#10637=AXIS2_PLACEMENT_3D('',#16894,#13291,#13292);
#10638=AXIS2_PLACEMENT_3D('',#16897,#13294,#13295);
#10639=AXIS2_PLACEMENT_3D('',#16898,#13296,#13297);
#10640=AXIS2_PLACEMENT_3D('',#16899,#13298,#13299);
#10641=AXIS2_PLACEMENT_3D('',#16900,#13300,#13301);
#10642=AXIS2_PLACEMENT_3D('',#16901,#13302,#13303);
#10643=AXIS2_PLACEMENT_3D('',#16903,#13304,#13305);
#10644=AXIS2_PLACEMENT_3D('',#16906,#13307,#13308);
#10645=AXIS2_PLACEMENT_3D('',#16907,#13309,#13310);
#10646=AXIS2_PLACEMENT_3D('',#16909,#13311,#13312);
#10647=AXIS2_PLACEMENT_3D('',#16912,#13314,#13315);
#10648=AXIS2_PLACEMENT_3D('',#16913,#13316,#13317);
#10649=AXIS2_PLACEMENT_3D('',#16914,#13318,#13319);
#10650=AXIS2_PLACEMENT_3D('',#16915,#13320,#13321);
#10651=AXIS2_PLACEMENT_3D('',#16916,#13322,#13323);
#10652=AXIS2_PLACEMENT_3D('',#16918,#13324,#13325);
#10653=AXIS2_PLACEMENT_3D('',#16921,#13327,#13328);
#10654=AXIS2_PLACEMENT_3D('',#16922,#13329,#13330);
#10655=AXIS2_PLACEMENT_3D('',#16924,#13331,#13332);
#10656=AXIS2_PLACEMENT_3D('',#16927,#13334,#13335);
#10657=AXIS2_PLACEMENT_3D('',#16928,#13336,#13337);
#10658=AXIS2_PLACEMENT_3D('',#16929,#13338,#13339);
#10659=AXIS2_PLACEMENT_3D('',#16930,#13340,#13341);
#10660=AXIS2_PLACEMENT_3D('',#16931,#13342,#13343);
#10661=AXIS2_PLACEMENT_3D('',#16932,#13344,#13345);
#10662=AXIS2_PLACEMENT_3D('',#16935,#13346,#13347);
#10663=AXIS2_PLACEMENT_3D('',#16941,#13351,#13352);
#10664=AXIS2_PLACEMENT_3D('',#16947,#13356,#13357);
#10665=AXIS2_PLACEMENT_3D('',#16949,#13358,#13359);
#10666=AXIS2_PLACEMENT_3D('',#16953,#13362,#13363);
#10667=AXIS2_PLACEMENT_3D('',#16956,#13366,#13367);
#10668=AXIS2_PLACEMENT_3D('',#16957,#13368,#13369);
#10669=AXIS2_PLACEMENT_3D('',#16959,#13370,#13371);
#10670=AXIS2_PLACEMENT_3D('',#16961,#13372,#13373);
#10671=AXIS2_PLACEMENT_3D('',#16962,#13374,#13375);
#10672=AXIS2_PLACEMENT_3D('',#16964,#13376,#13377);
#10673=AXIS2_PLACEMENT_3D('',#16966,#13379,#13380);
#10674=AXIS2_PLACEMENT_3D('',#16968,#13381,#13382);
#10675=AXIS2_PLACEMENT_3D('',#16969,#13383,#13384);
#10676=AXIS2_PLACEMENT_3D('',#16971,#13385,#13386);
#10677=AXIS2_PLACEMENT_3D('',#16973,#13388,#13389);
#10678=AXIS2_PLACEMENT_3D('',#16975,#13390,#13391);
#10679=AXIS2_PLACEMENT_3D('',#16976,#13392,#13393);
#10680=AXIS2_PLACEMENT_3D('',#16978,#13394,#13395);
#10681=AXIS2_PLACEMENT_3D('',#16980,#13397,#13398);
#10682=AXIS2_PLACEMENT_3D('',#16982,#13399,#13400);
#10683=AXIS2_PLACEMENT_3D('',#16983,#13401,#13402);
#10684=AXIS2_PLACEMENT_3D('',#16985,#13403,#13404);
#10685=AXIS2_PLACEMENT_3D('',#16987,#13406,#13407);
#10686=AXIS2_PLACEMENT_3D('',#16989,#13408,#13409);
#10687=AXIS2_PLACEMENT_3D('',#16990,#13410,#13411);
#10688=AXIS2_PLACEMENT_3D('',#16992,#13412,#13413);
#10689=AXIS2_PLACEMENT_3D('',#16994,#13415,#13416);
#10690=AXIS2_PLACEMENT_3D('',#16996,#13417,#13418);
#10691=AXIS2_PLACEMENT_3D('',#16997,#13419,#13420);
#10692=AXIS2_PLACEMENT_3D('',#16999,#13422,#13423);
#10693=AXIS2_PLACEMENT_3D('',#17000,#13424,#13425);
#10694=AXIS2_PLACEMENT_3D('',#17003,#13426,#13427);
#10695=AXIS2_PLACEMENT_3D('',#17007,#13429,#13430);
#10696=AXIS2_PLACEMENT_3D('',#17009,#13432,#13433);
#10697=AXIS2_PLACEMENT_3D('',#17015,#13437,#13438);
#10698=AXIS2_PLACEMENT_3D('',#17017,#13439,#13440);
#10699=AXIS2_PLACEMENT_3D('',#17019,#13441,#13442);
#10700=AXIS2_PLACEMENT_3D('',#17021,#13444,#13445);
#10701=AXIS2_PLACEMENT_3D('',#17024,#13448,#13449);
#10702=AXIS2_PLACEMENT_3D('',#17026,#13450,#13451);
#10703=AXIS2_PLACEMENT_3D('',#17028,#13452,#13453);
#10704=AXIS2_PLACEMENT_3D('',#17029,#13454,#13455);
#10705=AXIS2_PLACEMENT_3D('',#17031,#13456,#13457);
#10706=AXIS2_PLACEMENT_3D('',#17033,#13459,#13460);
#10707=AXIS2_PLACEMENT_3D('',#17035,#13461,#13462);
#10708=AXIS2_PLACEMENT_3D('',#17036,#13463,#13464);
#10709=AXIS2_PLACEMENT_3D('',#17038,#13466,#13467);
#10710=AXIS2_PLACEMENT_3D('',#17039,#13468,#13469);
#10711=AXIS2_PLACEMENT_3D('',#17040,#13470,#13471);
#10712=AXIS2_PLACEMENT_3D('',#17041,#13472,#13473);
#10713=AXIS2_PLACEMENT_3D('',#17050,#13478,#13479);
#10714=AXIS2_PLACEMENT_3D('',#17056,#13483,#13484);
#10715=AXIS2_PLACEMENT_3D('',#17062,#13488,#13489);
#10716=AXIS2_PLACEMENT_3D('',#17068,#13493,#13494);
#10717=AXIS2_PLACEMENT_3D('',#17074,#13498,#13499);
#10718=AXIS2_PLACEMENT_3D('',#17077,#13502,#13503);
#10719=AXIS2_PLACEMENT_3D('',#17078,#13504,#13505);
#10720=AXIS2_PLACEMENT_3D('',#17079,#13506,#13507);
#10721=AXIS2_PLACEMENT_3D('',#17081,#13508,#13509);
#10722=AXIS2_PLACEMENT_3D('',#17082,#13510,#13511);
#10723=AXIS2_PLACEMENT_3D('',#17084,#13512,#13513);
#10724=AXIS2_PLACEMENT_3D('',#17085,#13514,#13515);
#10725=AXIS2_PLACEMENT_3D('',#17087,#13516,#13517);
#10726=AXIS2_PLACEMENT_3D('',#17089,#13519,#13520);
#10727=AXIS2_PLACEMENT_3D('',#17091,#13521,#13522);
#10728=AXIS2_PLACEMENT_3D('',#17093,#13524,#13525);
#10729=AXIS2_PLACEMENT_3D('',#17095,#13526,#13527);
#10730=AXIS2_PLACEMENT_3D('',#17097,#13529,#13530);
#10731=AXIS2_PLACEMENT_3D('',#17099,#13531,#13532);
#10732=AXIS2_PLACEMENT_3D('',#17100,#13533,#13534);
#10733=AXIS2_PLACEMENT_3D('',#17102,#13535,#13536);
#10734=AXIS2_PLACEMENT_3D('',#17104,#13538,#13539);
#10735=AXIS2_PLACEMENT_3D('',#17106,#13541,#13542);
#10736=AXIS2_PLACEMENT_3D('',#17107,#13543,#13544);
#10737=AXIS2_PLACEMENT_3D('',#17108,#13545,#13546);
#10738=AXIS2_PLACEMENT_3D('',#17109,#13547,#13548);
#10739=AXIS2_PLACEMENT_3D('',#17110,#13549,#13550);
#10740=AXIS2_PLACEMENT_3D('',#17111,#13551,#13552);
#10741=AXIS2_PLACEMENT_3D('',#17112,#13553,#13554);
#10742=AXIS2_PLACEMENT_3D('',#17113,#13555,#13556);
#10743=AXIS2_PLACEMENT_3D('',#17114,#13557,#13558);
#10744=AXIS2_PLACEMENT_3D('',#17115,#13559,#13560);
#10745=AXIS2_PLACEMENT_3D('',#17116,#13561,#13562);
#10746=AXIS2_PLACEMENT_3D('',#17117,#13563,#13564);
#10747=AXIS2_PLACEMENT_3D('',#17118,#13565,#13566);
#10748=AXIS2_PLACEMENT_3D('',#17119,#13567,#13568);
#10749=AXIS2_PLACEMENT_3D('',#17120,#13569,#13570);
#10750=AXIS2_PLACEMENT_3D('',#17121,#13571,#13572);
#10751=AXIS2_PLACEMENT_3D('',#17122,#13573,#13574);
#10752=AXIS2_PLACEMENT_3D('',#17123,#13575,#13576);
#10753=AXIS2_PLACEMENT_3D('',#17124,#13577,#13578);
#10754=AXIS2_PLACEMENT_3D('',#17125,#13579,#13580);
#10755=AXIS2_PLACEMENT_3D('',#17126,#13581,#13582);
#10756=AXIS2_PLACEMENT_3D('',#17127,#13583,#13584);
#10757=AXIS2_PLACEMENT_3D('',#17128,#13585,#13586);
#10758=AXIS2_PLACEMENT_3D('',#17129,#13587,#13588);
#10759=AXIS2_PLACEMENT_3D('',#17130,#13589,#13590);
#10760=AXIS2_PLACEMENT_3D('',#17131,#13591,#13592);
#10761=AXIS2_PLACEMENT_3D('',#17132,#13593,#13594);
#10762=AXIS2_PLACEMENT_3D('',#17133,#13595,#13596);
#10763=AXIS2_PLACEMENT_3D('',#17134,#13597,#13598);
#10764=AXIS2_PLACEMENT_3D('',#17135,#13599,#13600);
#10765=AXIS2_PLACEMENT_3D('',#17136,#13601,#13602);
#10766=AXIS2_PLACEMENT_3D('',#17137,#13603,#13604);
#10767=AXIS2_PLACEMENT_3D('',#17138,#13605,#13606);
#10768=AXIS2_PLACEMENT_3D('',#17139,#13607,#13608);
#10769=AXIS2_PLACEMENT_3D('',#17140,#13609,#13610);
#10770=AXIS2_PLACEMENT_3D('',#17141,#13611,#13612);
#10771=AXIS2_PLACEMENT_3D('',#17142,#13613,#13614);
#10772=AXIS2_PLACEMENT_3D('',#17143,#13615,#13616);
#10773=AXIS2_PLACEMENT_3D('',#17144,#13617,#13618);
#10774=AXIS2_PLACEMENT_3D('',#17145,#13619,#13620);
#10775=AXIS2_PLACEMENT_3D('',#17146,#13621,#13622);
#10776=AXIS2_PLACEMENT_3D('',#17147,#13623,#13624);
#10777=AXIS2_PLACEMENT_3D('',#17148,#13625,#13626);
#10778=AXIS2_PLACEMENT_3D('',#17149,#13627,#13628);
#10779=AXIS2_PLACEMENT_3D('',#17150,#13629,#13630);
#10780=AXIS2_PLACEMENT_3D('',#17151,#13631,#13632);
#10781=AXIS2_PLACEMENT_3D('',#17152,#13633,#13634);
#10782=AXIS2_PLACEMENT_3D('',#17153,#13635,#13636);
#10783=AXIS2_PLACEMENT_3D('',#17154,#13637,#13638);
#10784=AXIS2_PLACEMENT_3D('',#17155,#13639,#13640);
#10785=AXIS2_PLACEMENT_3D('',#17156,#13641,#13642);
#10786=AXIS2_PLACEMENT_3D('',#17157,#13643,#13644);
#10787=AXIS2_PLACEMENT_3D('',#17158,#13645,#13646);
#10788=AXIS2_PLACEMENT_3D('',#17159,#13647,#13648);
#10789=AXIS2_PLACEMENT_3D('',#17160,#13649,#13650);
#10790=AXIS2_PLACEMENT_3D('',#17161,#13651,#13652);
#10791=AXIS2_PLACEMENT_3D('',#17162,#13653,#13654);
#10792=AXIS2_PLACEMENT_3D('',#17163,#13655,#13656);
#10793=AXIS2_PLACEMENT_3D('',#17164,#13657,#13658);
#10794=AXIS2_PLACEMENT_3D('',#17165,#13659,#13660);
#10795=AXIS2_PLACEMENT_3D('',#17166,#13661,#13662);
#10796=AXIS2_PLACEMENT_3D('',#17167,#13663,#13664);
#10797=AXIS2_PLACEMENT_3D('',#17168,#13665,#13666);
#10798=AXIS2_PLACEMENT_3D('',#17169,#13667,#13668);
#10799=AXIS2_PLACEMENT_3D('',#17170,#13669,#13670);
#10800=AXIS2_PLACEMENT_3D('',#17171,#13671,#13672);
#10801=AXIS2_PLACEMENT_3D('',#17172,#13673,#13674);
#10802=AXIS2_PLACEMENT_3D('',#17173,#13675,#13676);
#10803=AXIS2_PLACEMENT_3D('',#17174,#13677,#13678);
#10804=AXIS2_PLACEMENT_3D('',#17175,#13679,#13680);
#10805=AXIS2_PLACEMENT_3D('',#17176,#13681,#13682);
#10806=AXIS2_PLACEMENT_3D('',#17177,#13683,#13684);
#10807=AXIS2_PLACEMENT_3D('',#17178,#13685,#13686);
#10808=AXIS2_PLACEMENT_3D('',#17179,#13687,#13688);
#10809=AXIS2_PLACEMENT_3D('',#17180,#13689,#13690);
#10810=AXIS2_PLACEMENT_3D('',#17181,#13691,#13692);
#10811=AXIS2_PLACEMENT_3D('',#17182,#13693,#13694);
#10812=AXIS2_PLACEMENT_3D('',#17183,#13695,#13696);
#10813=AXIS2_PLACEMENT_3D('',#17184,#13697,#13698);
#10814=AXIS2_PLACEMENT_3D('',#17185,#13699,#13700);
#10815=AXIS2_PLACEMENT_3D('',#17186,#13701,#13702);
#10816=AXIS2_PLACEMENT_3D('',#17187,#13703,#13704);
#10817=AXIS2_PLACEMENT_3D('',#17188,#13705,#13706);
#10818=AXIS2_PLACEMENT_3D('',#17189,#13707,#13708);
#10819=AXIS2_PLACEMENT_3D('',#17190,#13709,#13710);
#10820=AXIS2_PLACEMENT_3D('',#17191,#13711,#13712);
#10821=AXIS2_PLACEMENT_3D('',#17192,#13713,#13714);
#10822=AXIS2_PLACEMENT_3D('',#17193,#13715,#13716);
#10823=AXIS2_PLACEMENT_3D('',#17194,#13717,#13718);
#10824=AXIS2_PLACEMENT_3D('',#17195,#13719,#13720);
#10825=AXIS2_PLACEMENT_3D('',#17196,#13721,#13722);
#10826=AXIS2_PLACEMENT_3D('',#17197,#13723,#13724);
#10827=AXIS2_PLACEMENT_3D('',#17198,#13725,#13726);
#10828=AXIS2_PLACEMENT_3D('',#17199,#13727,#13728);
#10829=AXIS2_PLACEMENT_3D('',#17200,#13729,#13730);
#10830=DIRECTION('axis',(0.,0.,1.));
#10831=DIRECTION('refdir',(1.,0.,0.));
#10832=DIRECTION('axis',(0.,0.,1.));
#10833=DIRECTION('refdir',(1.,0.,0.));
#10834=DIRECTION('axis',(0.,0.,1.));
#10835=DIRECTION('refdir',(1.,0.,0.));
#10836=DIRECTION('center_axis',(0.,0.,1.));
#10837=DIRECTION('ref_axis',(1.,0.,0.));
#10838=DIRECTION('center_axis',(0.,0.,1.));
#10839=DIRECTION('ref_axis',(1.,0.,0.));
#10840=DIRECTION('',(0.,0.,1.));
#10841=DIRECTION('center_axis',(0.,0.,-1.));
#10842=DIRECTION('ref_axis',(1.,0.,0.));
#10843=DIRECTION('center_axis',(0.,0.,1.));
#10844=DIRECTION('ref_axis',(1.,0.,0.));
#10845=DIRECTION('center_axis',(0.,0.,1.));
#10846=DIRECTION('ref_axis',(1.,0.,0.));
#10847=DIRECTION('',(0.,0.,1.));
#10848=DIRECTION('center_axis',(0.,0.,-1.));
#10849=DIRECTION('ref_axis',(1.,0.,0.));
#10850=DIRECTION('center_axis',(0.,0.,1.));
#10851=DIRECTION('ref_axis',(1.,0.,0.));
#10852=DIRECTION('center_axis',(0.,0.,1.));
#10853=DIRECTION('ref_axis',(1.,0.,0.));
#10854=DIRECTION('',(0.,0.,1.));
#10855=DIRECTION('center_axis',(0.,0.,-1.));
#10856=DIRECTION('ref_axis',(1.,0.,0.));
#10857=DIRECTION('center_axis',(0.,0.,1.));
#10858=DIRECTION('ref_axis',(1.,0.,0.));
#10859=DIRECTION('center_axis',(0.,0.,1.));
#10860=DIRECTION('ref_axis',(1.,0.,0.));
#10861=DIRECTION('',(0.,0.,1.));
#10862=DIRECTION('center_axis',(0.,0.,-1.));
#10863=DIRECTION('ref_axis',(1.,0.,0.));
#10864=DIRECTION('center_axis',(0.,0.,1.));
#10865=DIRECTION('ref_axis',(1.,0.,0.));
#10866=DIRECTION('center_axis',(0.,0.,1.));
#10867=DIRECTION('ref_axis',(1.,0.,0.));
#10868=DIRECTION('',(0.,0.,1.));
#10869=DIRECTION('center_axis',(0.,0.,-1.));
#10870=DIRECTION('ref_axis',(1.,0.,0.));
#10871=DIRECTION('center_axis',(0.,0.,1.));
#10872=DIRECTION('ref_axis',(1.,0.,0.));
#10873=DIRECTION('center_axis',(0.,0.,1.));
#10874=DIRECTION('ref_axis',(1.,0.,0.));
#10875=DIRECTION('',(0.,0.,1.));
#10876=DIRECTION('center_axis',(0.,0.,-1.));
#10877=DIRECTION('ref_axis',(1.,0.,0.));
#10878=DIRECTION('center_axis',(0.,0.,1.));
#10879=DIRECTION('ref_axis',(1.,0.,0.));
#10880=DIRECTION('center_axis',(0.,0.,1.));
#10881=DIRECTION('ref_axis',(1.,0.,0.));
#10882=DIRECTION('',(0.,0.,1.));
#10883=DIRECTION('center_axis',(0.,0.,-1.));
#10884=DIRECTION('ref_axis',(1.,0.,0.));
#10885=DIRECTION('center_axis',(0.,0.,1.));
#10886=DIRECTION('ref_axis',(1.,0.,0.));
#10887=DIRECTION('center_axis',(0.,0.,1.));
#10888=DIRECTION('ref_axis',(1.,0.,0.));
#10889=DIRECTION('',(0.,0.,1.));
#10890=DIRECTION('center_axis',(0.,0.,-1.));
#10891=DIRECTION('ref_axis',(1.,0.,0.));
#10892=DIRECTION('center_axis',(0.,0.,1.));
#10893=DIRECTION('ref_axis',(1.,0.,0.));
#10894=DIRECTION('center_axis',(0.,0.,1.));
#10895=DIRECTION('ref_axis',(1.,0.,0.));
#10896=DIRECTION('',(0.,0.,1.));
#10897=DIRECTION('center_axis',(0.,0.,-1.));
#10898=DIRECTION('ref_axis',(1.,0.,0.));
#10899=DIRECTION('center_axis',(0.,0.,1.));
#10900=DIRECTION('ref_axis',(1.,0.,0.));
#10901=DIRECTION('center_axis',(0.,0.,1.));
#10902=DIRECTION('ref_axis',(1.,0.,0.));
#10903=DIRECTION('',(0.,0.,1.));
#10904=DIRECTION('center_axis',(0.,0.,-1.));
#10905=DIRECTION('ref_axis',(1.,0.,0.));
#10906=DIRECTION('center_axis',(0.,0.,1.));
#10907=DIRECTION('ref_axis',(1.,0.,0.));
#10908=DIRECTION('center_axis',(0.,0.,1.));
#10909=DIRECTION('ref_axis',(1.,0.,0.));
#10910=DIRECTION('',(0.,0.,1.));
#10911=DIRECTION('center_axis',(0.,0.,-1.));
#10912=DIRECTION('ref_axis',(1.,0.,0.));
#10913=DIRECTION('center_axis',(0.,0.,1.));
#10914=DIRECTION('ref_axis',(1.,0.,0.));
#10915=DIRECTION('center_axis',(0.,0.,1.));
#10916=DIRECTION('ref_axis',(1.,0.,0.));
#10917=DIRECTION('',(0.,0.,1.));
#10918=DIRECTION('center_axis',(0.,0.,-1.));
#10919=DIRECTION('ref_axis',(1.,0.,0.));
#10920=DIRECTION('center_axis',(0.,1.,0.));
#10921=DIRECTION('ref_axis',(-1.,0.,0.));
#10922=DIRECTION('',(-1.,0.,0.));
#10923=DIRECTION('',(0.,0.,1.));
#10924=DIRECTION('',(-1.,0.,0.));
#10925=DIRECTION('',(0.,0.,1.));
#10926=DIRECTION('center_axis',(1.,0.,0.));
#10927=DIRECTION('ref_axis',(0.,1.,0.));
#10928=DIRECTION('',(0.,1.,0.));
#10929=DIRECTION('',(0.,1.,0.));
#10930=DIRECTION('',(0.,0.,1.));
#10931=DIRECTION('center_axis',(0.,-1.,0.));
#10932=DIRECTION('ref_axis',(1.,0.,0.));
#10933=DIRECTION('',(1.,0.,0.));
#10934=DIRECTION('',(1.,0.,0.));
#10935=DIRECTION('',(0.,0.,1.));
#10936=DIRECTION('center_axis',(-1.,0.,0.));
#10937=DIRECTION('ref_axis',(0.,-1.,0.));
#10938=DIRECTION('',(0.,-1.,0.));
#10939=DIRECTION('',(0.,-1.,0.));
#10940=DIRECTION('center_axis',(0.,0.,1.));
#10941=DIRECTION('ref_axis',(1.,0.,0.));
#10942=DIRECTION('center_axis',(0.,0.,1.));
#10943=DIRECTION('ref_axis',(1.,0.,0.));
#10944=DIRECTION('axis',(0.,0.,1.));
#10945=DIRECTION('refdir',(1.,0.,0.));
#10946=DIRECTION('center_axis',(0.,0.,1.));
#10947=DIRECTION('ref_axis',(1.,0.,0.));
#10948=DIRECTION('center_axis',(0.,0.,1.));
#10949=DIRECTION('ref_axis',(1.,0.,0.));
#10950=DIRECTION('',(0.,0.,1.));
#10951=DIRECTION('center_axis',(0.,0.,-1.));
#10952=DIRECTION('ref_axis',(1.,0.,0.));
#10953=DIRECTION('center_axis',(0.,0.,1.));
#10954=DIRECTION('ref_axis',(1.,0.,0.));
#10955=DIRECTION('center_axis',(0.,0.,1.));
#10956=DIRECTION('ref_axis',(1.,0.,0.));
#10957=DIRECTION('center_axis',(0.,0.,1.));
#10958=DIRECTION('ref_axis',(1.,0.,0.));
#10959=DIRECTION('',(0.,0.,1.));
#10960=DIRECTION('center_axis',(0.,0.,-1.));
#10961=DIRECTION('ref_axis',(1.,0.,0.));
#10962=DIRECTION('center_axis',(0.,0.,1.));
#10963=DIRECTION('ref_axis',(1.,0.,0.));
#10964=DIRECTION('center_axis',(0.,0.,1.));
#10965=DIRECTION('ref_axis',(1.,0.,0.));
#10966=DIRECTION('center_axis',(0.,0.,1.));
#10967=DIRECTION('ref_axis',(1.,0.,0.));
#10968=DIRECTION('',(0.,0.,1.));
#10969=DIRECTION('center_axis',(0.,0.,-1.));
#10970=DIRECTION('ref_axis',(1.,0.,0.));
#10971=DIRECTION('center_axis',(0.,0.,1.));
#10972=DIRECTION('ref_axis',(1.,0.,0.));
#10973=DIRECTION('center_axis',(0.,0.,1.));
#10974=DIRECTION('ref_axis',(1.,0.,0.));
#10975=DIRECTION('center_axis',(0.,0.,1.));
#10976=DIRECTION('ref_axis',(1.,0.,0.));
#10977=DIRECTION('center_axis',(0.,0.,1.));
#10978=DIRECTION('ref_axis',(1.,0.,0.));
#10979=DIRECTION('',(0.,0.,1.));
#10980=DIRECTION('center_axis',(0.,0.,-1.));
#10981=DIRECTION('ref_axis',(1.,0.,0.));
#10982=DIRECTION('center_axis',(0.,0.,1.));
#10983=DIRECTION('ref_axis',(1.,0.,0.));
#10984=DIRECTION('center_axis',(0.,0.,1.));
#10985=DIRECTION('ref_axis',(1.,0.,0.));
#10986=DIRECTION('center_axis',(0.,0.,1.));
#10987=DIRECTION('ref_axis',(1.,0.,0.));
#10988=DIRECTION('center_axis',(0.,0.,1.));
#10989=DIRECTION('ref_axis',(1.,0.,0.));
#10990=DIRECTION('',(0.,0.,1.));
#10991=DIRECTION('center_axis',(0.,0.,-1.));
#10992=DIRECTION('ref_axis',(1.,0.,0.));
#10993=DIRECTION('center_axis',(0.,0.,1.));
#10994=DIRECTION('ref_axis',(1.,0.,0.));
#10995=DIRECTION('center_axis',(0.,0.,1.));
#10996=DIRECTION('ref_axis',(1.,0.,0.));
#10997=DIRECTION('center_axis',(0.,0.,1.));
#10998=DIRECTION('ref_axis',(1.,0.,0.));
#10999=DIRECTION('center_axis',(0.,0.,1.));
#11000=DIRECTION('ref_axis',(1.,0.,0.));
#11001=DIRECTION('',(0.,0.,1.));
#11002=DIRECTION('center_axis',(0.,0.,-1.));
#11003=DIRECTION('ref_axis',(1.,0.,0.));
#11004=DIRECTION('center_axis',(0.,0.,1.));
#11005=DIRECTION('ref_axis',(1.,0.,0.));
#11006=DIRECTION('center_axis',(0.,0.,1.));
#11007=DIRECTION('ref_axis',(1.,0.,0.));
#11008=DIRECTION('center_axis',(0.,0.,1.));
#11009=DIRECTION('ref_axis',(1.,0.,0.));
#11010=DIRECTION('center_axis',(0.,0.,1.));
#11011=DIRECTION('ref_axis',(1.,0.,0.));
#11012=DIRECTION('',(0.,0.,1.));
#11013=DIRECTION('center_axis',(0.,0.,1.));
#11014=DIRECTION('ref_axis',(1.,0.,0.));
#11015=DIRECTION('center_axis',(0.,0.,1.));
#11016=DIRECTION('ref_axis',(1.,0.,0.));
#11017=DIRECTION('',(0.,0.,1.));
#11018=DIRECTION('center_axis',(0.,0.,1.));
#11019=DIRECTION('ref_axis',(1.,0.,0.));
#11020=DIRECTION('center_axis',(0.,0.,1.));
#11021=DIRECTION('ref_axis',(1.,0.,0.));
#11022=DIRECTION('',(0.,0.,1.));
#11023=DIRECTION('center_axis',(0.,0.,1.));
#11024=DIRECTION('ref_axis',(1.,0.,0.));
#11025=DIRECTION('center_axis',(0.,0.,1.));
#11026=DIRECTION('ref_axis',(1.,0.,0.));
#11027=DIRECTION('',(0.,0.,1.));
#11028=DIRECTION('center_axis',(0.,1.,0.));
#11029=DIRECTION('ref_axis',(-1.,0.,0.));
#11030=DIRECTION('',(-1.,0.,0.));
#11031=DIRECTION('',(0.,0.,1.));
#11032=DIRECTION('',(-1.,0.,0.));
#11033=DIRECTION('',(0.,0.,1.));
#11034=DIRECTION('center_axis',(1.,0.,0.));
#11035=DIRECTION('ref_axis',(0.,1.,0.));
#11036=DIRECTION('',(0.,1.,0.));
#11037=DIRECTION('',(0.,1.,0.));
#11038=DIRECTION('',(0.,0.,1.));
#11039=DIRECTION('center_axis',(0.,-1.,0.));
#11040=DIRECTION('ref_axis',(1.,0.,0.));
#11041=DIRECTION('',(1.,0.,0.));
#11042=DIRECTION('',(1.,0.,0.));
#11043=DIRECTION('',(0.,0.,1.));
#11044=DIRECTION('center_axis',(-1.,0.,0.));
#11045=DIRECTION('ref_axis',(0.,-1.,0.));
#11046=DIRECTION('',(0.,-1.,0.));
#11047=DIRECTION('',(0.,-1.,0.));
#11048=DIRECTION('center_axis',(0.,0.,1.));
#11049=DIRECTION('ref_axis',(1.,0.,0.));
#11050=DIRECTION('center_axis',(0.,0.,1.));
#11051=DIRECTION('ref_axis',(1.,0.,0.));
#11052=DIRECTION('axis',(0.,0.,1.));
#11053=DIRECTION('refdir',(1.,0.,0.));
#11054=DIRECTION('center_axis',(0.,0.,1.));
#11055=DIRECTION('ref_axis',(1.,0.,0.));
#11056=DIRECTION('center_axis',(0.,0.,-1.));
#11057=DIRECTION('ref_axis',(1.,0.,0.));
#11058=DIRECTION('',(0.,0.,-1.));
#11059=DIRECTION('center_axis',(0.,0.,-1.));
#11060=DIRECTION('ref_axis',(1.,0.,0.));
#11061=DIRECTION('center_axis',(0.,0.,1.));
#11062=DIRECTION('ref_axis',(1.,0.,0.));
#11063=DIRECTION('center_axis',(0.,0.,1.));
#11064=DIRECTION('ref_axis',(1.,0.,0.));
#11065=DIRECTION('',(0.,0.,-1.));
#11066=DIRECTION('center_axis',(0.,0.,1.));
#11067=DIRECTION('ref_axis',(1.,0.,0.));
#11068=DIRECTION('center_axis',(0.,0.,1.));
#11069=DIRECTION('ref_axis',(1.,0.,0.));
#11070=DIRECTION('center_axis',(0.,0.,1.));
#11071=DIRECTION('ref_axis',(1.,0.,0.));
#11072=DIRECTION('axis',(0.,0.,1.));
#11073=DIRECTION('refdir',(1.,0.,0.));
#11074=DIRECTION('center_axis',(0.,0.,1.));
#11075=DIRECTION('ref_axis',(1.,0.,0.));
#11076=DIRECTION('center_axis',(0.,0.,-1.));
#11077=DIRECTION('ref_axis',(1.,0.,0.));
#11078=DIRECTION('',(0.,0.,-1.));
#11079=DIRECTION('center_axis',(0.,0.,-1.));
#11080=DIRECTION('ref_axis',(1.,0.,0.));
#11081=DIRECTION('center_axis',(0.,0.,1.));
#11082=DIRECTION('ref_axis',(1.,0.,0.));
#11083=DIRECTION('center_axis',(0.,0.,1.));
#11084=DIRECTION('ref_axis',(1.,0.,0.));
#11085=DIRECTION('',(0.,0.,-1.));
#11086=DIRECTION('center_axis',(0.,0.,1.));
#11087=DIRECTION('ref_axis',(1.,0.,0.));
#11088=DIRECTION('center_axis',(0.,0.,1.));
#11089=DIRECTION('ref_axis',(1.,0.,0.));
#11090=DIRECTION('center_axis',(0.,0.,1.));
#11091=DIRECTION('ref_axis',(1.,0.,0.));
#11092=DIRECTION('axis',(0.,0.,1.));
#11093=DIRECTION('refdir',(1.,0.,0.));
#11094=DIRECTION('center_axis',(0.,0.,1.));
#11095=DIRECTION('ref_axis',(1.,0.,0.));
#11096=DIRECTION('center_axis',(0.,0.,1.));
#11097=DIRECTION('ref_axis',(1.,0.,0.));
#11098=DIRECTION('',(0.,0.,1.));
#11099=DIRECTION('center_axis',(0.,0.,-1.));
#11100=DIRECTION('ref_axis',(1.,0.,0.));
#11101=DIRECTION('center_axis',(0.,0.,1.));
#11102=DIRECTION('ref_axis',(1.,0.,0.));
#11103=DIRECTION('center_axis',(0.,0.,1.));
#11104=DIRECTION('ref_axis',(1.,0.,0.));
#11105=DIRECTION('center_axis',(0.,0.,1.));
#11106=DIRECTION('ref_axis',(1.,0.,0.));
#11107=DIRECTION('',(0.,0.,1.));
#11108=DIRECTION('center_axis',(0.,0.,-1.));
#11109=DIRECTION('ref_axis',(1.,0.,0.));
#11110=DIRECTION('center_axis',(0.,0.,1.));
#11111=DIRECTION('ref_axis',(1.,0.,0.));
#11112=DIRECTION('center_axis',(0.,0.,1.));
#11113=DIRECTION('ref_axis',(1.,0.,0.));
#11114=DIRECTION('center_axis',(0.,0.,1.));
#11115=DIRECTION('ref_axis',(1.,0.,0.));
#11116=DIRECTION('',(0.,0.,1.));
#11117=DIRECTION('center_axis',(0.,0.,-1.));
#11118=DIRECTION('ref_axis',(1.,0.,0.));
#11119=DIRECTION('center_axis',(0.,0.,1.));
#11120=DIRECTION('ref_axis',(1.,0.,0.));
#11121=DIRECTION('center_axis',(0.,0.,1.));
#11122=DIRECTION('ref_axis',(1.,0.,0.));
#11123=DIRECTION('center_axis',(0.,0.,1.));
#11124=DIRECTION('ref_axis',(1.,0.,0.));
#11125=DIRECTION('center_axis',(0.,0.,1.));
#11126=DIRECTION('ref_axis',(1.,0.,0.));
#11127=DIRECTION('',(0.,0.,1.));
#11128=DIRECTION('center_axis',(0.,0.,-1.));
#11129=DIRECTION('ref_axis',(1.,0.,0.));
#11130=DIRECTION('center_axis',(0.,0.,1.));
#11131=DIRECTION('ref_axis',(1.,0.,0.));
#11132=DIRECTION('center_axis',(0.,0.,1.));
#11133=DIRECTION('ref_axis',(1.,0.,0.));
#11134=DIRECTION('center_axis',(0.,0.,1.));
#11135=DIRECTION('ref_axis',(1.,0.,0.));
#11136=DIRECTION('center_axis',(0.,0.,1.));
#11137=DIRECTION('ref_axis',(1.,0.,0.));
#11138=DIRECTION('',(0.,0.,1.));
#11139=DIRECTION('center_axis',(0.,0.,-1.));
#11140=DIRECTION('ref_axis',(1.,0.,0.));
#11141=DIRECTION('center_axis',(0.,0.,1.));
#11142=DIRECTION('ref_axis',(1.,0.,0.));
#11143=DIRECTION('center_axis',(0.,0.,1.));
#11144=DIRECTION('ref_axis',(1.,0.,0.));
#11145=DIRECTION('center_axis',(0.,0.,1.));
#11146=DIRECTION('ref_axis',(1.,0.,0.));
#11147=DIRECTION('center_axis',(0.,0.,1.));
#11148=DIRECTION('ref_axis',(1.,0.,0.));
#11149=DIRECTION('',(0.,0.,1.));
#11150=DIRECTION('center_axis',(0.,0.,-1.));
#11151=DIRECTION('ref_axis',(1.,0.,0.));
#11152=DIRECTION('center_axis',(0.,0.,1.));
#11153=DIRECTION('ref_axis',(1.,0.,0.));
#11154=DIRECTION('center_axis',(0.,0.,1.));
#11155=DIRECTION('ref_axis',(1.,0.,0.));
#11156=DIRECTION('center_axis',(0.,0.,1.));
#11157=DIRECTION('ref_axis',(1.,0.,0.));
#11158=DIRECTION('center_axis',(0.,0.,1.));
#11159=DIRECTION('ref_axis',(1.,0.,0.));
#11160=DIRECTION('',(0.,0.,1.));
#11161=DIRECTION('center_axis',(0.,0.,1.));
#11162=DIRECTION('ref_axis',(1.,0.,0.));
#11163=DIRECTION('center_axis',(0.,0.,1.));
#11164=DIRECTION('ref_axis',(1.,0.,0.));
#11165=DIRECTION('',(0.,0.,1.));
#11166=DIRECTION('center_axis',(0.,0.,1.));
#11167=DIRECTION('ref_axis',(1.,0.,0.));
#11168=DIRECTION('center_axis',(0.,0.,1.));
#11169=DIRECTION('ref_axis',(1.,0.,0.));
#11170=DIRECTION('',(0.,0.,1.));
#11171=DIRECTION('center_axis',(0.,0.,1.));
#11172=DIRECTION('ref_axis',(1.,0.,0.));
#11173=DIRECTION('center_axis',(0.,0.,1.));
#11174=DIRECTION('ref_axis',(1.,0.,0.));
#11175=DIRECTION('',(0.,0.,1.));
#11176=DIRECTION('center_axis',(0.,1.,0.));
#11177=DIRECTION('ref_axis',(-1.,0.,0.));
#11178=DIRECTION('',(-1.,0.,0.));
#11179=DIRECTION('',(0.,0.,1.));
#11180=DIRECTION('',(-1.,0.,0.));
#11181=DIRECTION('',(0.,0.,1.));
#11182=DIRECTION('center_axis',(1.,0.,0.));
#11183=DIRECTION('ref_axis',(0.,1.,0.));
#11184=DIRECTION('',(0.,1.,0.));
#11185=DIRECTION('',(0.,1.,0.));
#11186=DIRECTION('',(0.,0.,1.));
#11187=DIRECTION('center_axis',(0.,-1.,0.));
#11188=DIRECTION('ref_axis',(1.,0.,0.));
#11189=DIRECTION('',(1.,0.,0.));
#11190=DIRECTION('',(1.,0.,0.));
#11191=DIRECTION('',(0.,0.,1.));
#11192=DIRECTION('center_axis',(-1.,0.,0.));
#11193=DIRECTION('ref_axis',(0.,-1.,0.));
#11194=DIRECTION('',(0.,-1.,0.));
#11195=DIRECTION('',(0.,-1.,0.));
#11196=DIRECTION('center_axis',(0.,0.,1.));
#11197=DIRECTION('ref_axis',(1.,0.,0.));
#11198=DIRECTION('center_axis',(0.,0.,1.));
#11199=DIRECTION('ref_axis',(1.,0.,0.));
#11200=DIRECTION('axis',(0.,0.,1.));
#11201=DIRECTION('refdir',(1.,0.,0.));
#11202=DIRECTION('center_axis',(0.,0.,1.));
#11203=DIRECTION('ref_axis',(1.,0.,0.));
#11204=DIRECTION('center_axis',(0.,0.,-1.));
#11205=DIRECTION('ref_axis',(1.,0.,0.));
#11206=DIRECTION('',(0.,0.,-1.));
#11207=DIRECTION('center_axis',(0.,0.,-1.));
#11208=DIRECTION('ref_axis',(1.,0.,0.));
#11209=DIRECTION('center_axis',(0.,0.,1.));
#11210=DIRECTION('ref_axis',(1.,0.,0.));
#11211=DIRECTION('center_axis',(0.,0.,1.));
#11212=DIRECTION('ref_axis',(1.,0.,0.));
#11213=DIRECTION('',(0.,0.,-1.));
#11214=DIRECTION('center_axis',(0.,0.,1.));
#11215=DIRECTION('ref_axis',(1.,0.,0.));
#11216=DIRECTION('center_axis',(0.,0.,1.));
#11217=DIRECTION('ref_axis',(1.,0.,0.));
#11218=DIRECTION('center_axis',(0.,0.,1.));
#11219=DIRECTION('ref_axis',(1.,0.,0.));
#11220=DIRECTION('axis',(0.,0.,1.));
#11221=DIRECTION('refdir',(1.,0.,0.));
#11222=DIRECTION('center_axis',(0.,0.,1.));
#11223=DIRECTION('ref_axis',(1.,0.,0.));
#11224=DIRECTION('center_axis',(0.,0.,-1.));
#11225=DIRECTION('ref_axis',(1.,0.,0.));
#11226=DIRECTION('',(0.,0.,-1.));
#11227=DIRECTION('center_axis',(0.,0.,-1.));
#11228=DIRECTION('ref_axis',(1.,0.,0.));
#11229=DIRECTION('center_axis',(0.,0.,1.));
#11230=DIRECTION('ref_axis',(1.,0.,0.));
#11231=DIRECTION('center_axis',(0.,0.,1.));
#11232=DIRECTION('ref_axis',(1.,0.,0.));
#11233=DIRECTION('',(0.,0.,-1.));
#11234=DIRECTION('center_axis',(0.,0.,1.));
#11235=DIRECTION('ref_axis',(1.,0.,0.));
#11236=DIRECTION('center_axis',(0.,0.,1.));
#11237=DIRECTION('ref_axis',(1.,0.,0.));
#11238=DIRECTION('center_axis',(0.,0.,1.));
#11239=DIRECTION('ref_axis',(1.,0.,0.));
#11240=DIRECTION('axis',(0.,0.,1.));
#11241=DIRECTION('refdir',(1.,0.,0.));
#11242=DIRECTION('center_axis',(0.,0.,1.));
#11243=DIRECTION('ref_axis',(1.,0.,0.));
#11244=DIRECTION('',(0.,0.,1.));
#11245=DIRECTION('center_axis',(0.,0.,1.));
#11246=DIRECTION('ref_axis',(1.,0.,0.));
#11247=DIRECTION('',(0.,0.,1.));
#11248=DIRECTION('center_axis',(0.,0.,-1.));
#11249=DIRECTION('ref_axis',(1.,0.,0.));
#11250=DIRECTION('center_axis',(0.,0.,1.));
#11251=DIRECTION('ref_axis',(1.,0.,0.));
#11252=DIRECTION('center_axis',(0.,0.,1.));
#11253=DIRECTION('ref_axis',(1.,0.,0.));
#11254=DIRECTION('',(0.,0.,1.));
#11255=DIRECTION('center_axis',(0.,0.,-1.));
#11256=DIRECTION('ref_axis',(1.,0.,0.));
#11257=DIRECTION('',(0.,0.,1.));
#11258=DIRECTION('center_axis',(0.,0.,1.));
#11259=DIRECTION('ref_axis',(1.,0.,0.));
#11260=DIRECTION('center_axis',(0.,0.,1.));
#11261=DIRECTION('ref_axis',(1.,0.,0.));
#11262=DIRECTION('center_axis',(0.,0.,1.));
#11263=DIRECTION('ref_axis',(1.,0.,0.));
#11264=DIRECTION('center_axis',(0.,0.,-1.));
#11265=DIRECTION('ref_axis',(1.,0.,0.));
#11266=DIRECTION('',(0.,0.,1.));
#11267=DIRECTION('center_axis',(0.,0.,1.));
#11268=DIRECTION('ref_axis',(1.,0.,0.));
#11269=DIRECTION('center_axis',(0.,0.,1.));
#11270=DIRECTION('ref_axis',(1.,0.,0.));
#11271=DIRECTION('center_axis',(0.,0.,1.));
#11272=DIRECTION('ref_axis',(1.,0.,0.));
#11273=DIRECTION('center_axis',(0.,0.,1.));
#11274=DIRECTION('ref_axis',(1.,0.,0.));
#11275=DIRECTION('',(0.,-1.,0.));
#11276=DIRECTION('',(0.,-1.,0.));
#11277=DIRECTION('',(1.,0.,0.));
#11278=DIRECTION('',(0.,1.,0.));
#11279=DIRECTION('',(0.,1.,0.));
#11280=DIRECTION('',(-1.,0.,0.));
#11281=DIRECTION('center_axis',(0.,0.,-1.));
#11282=DIRECTION('ref_axis',(1.,0.,0.));
#11283=DIRECTION('center_axis',(0.,0.,-1.));
#11284=DIRECTION('ref_axis',(1.,0.,0.));
#11285=DIRECTION('center_axis',(0.,0.,-1.));
#11286=DIRECTION('ref_axis',(1.,0.,0.));
#11287=DIRECTION('center_axis',(0.,0.,-1.));
#11288=DIRECTION('ref_axis',(1.,0.,0.));
#11289=DIRECTION('center_axis',(0.,0.,1.));
#11290=DIRECTION('ref_axis',(1.,0.,0.));
#11291=DIRECTION('center_axis',(0.,0.,1.));
#11292=DIRECTION('ref_axis',(1.,0.,0.));
#11293=DIRECTION('',(0.,0.,1.));
#11294=DIRECTION('center_axis',(0.,0.,1.));
#11295=DIRECTION('ref_axis',(1.,0.,0.));
#11296=DIRECTION('center_axis',(0.,0.,1.));
#11297=DIRECTION('ref_axis',(1.,0.,0.));
#11298=DIRECTION('',(0.,0.,1.));
#11299=DIRECTION('center_axis',(0.,0.,1.));
#11300=DIRECTION('ref_axis',(1.,0.,0.));
#11301=DIRECTION('center_axis',(0.,0.,1.));
#11302=DIRECTION('ref_axis',(1.,0.,0.));
#11303=DIRECTION('',(0.,0.,1.));
#11304=DIRECTION('center_axis',(0.,0.,1.));
#11305=DIRECTION('ref_axis',(1.,0.,0.));
#11306=DIRECTION('center_axis',(0.,0.,1.));
#11307=DIRECTION('ref_axis',(1.,0.,0.));
#11308=DIRECTION('center_axis',(0.,0.,1.));
#11309=DIRECTION('ref_axis',(1.,0.,0.));
#11310=DIRECTION('',(0.,0.,1.));
#11311=DIRECTION('center_axis',(0.,0.,1.));
#11312=DIRECTION('ref_axis',(1.,0.,0.));
#11313=DIRECTION('center_axis',(0.,0.,1.));
#11314=DIRECTION('ref_axis',(1.,0.,0.));
#11315=DIRECTION('center_axis',(0.,0.,1.));
#11316=DIRECTION('ref_axis',(1.,0.,0.));
#11317=DIRECTION('',(0.,0.,1.));
#11318=DIRECTION('center_axis',(0.,0.,1.));
#11319=DIRECTION('ref_axis',(1.,0.,0.));
#11320=DIRECTION('center_axis',(0.,0.,1.));
#11321=DIRECTION('ref_axis',(1.,0.,0.));
#11322=DIRECTION('center_axis',(0.,0.,1.));
#11323=DIRECTION('ref_axis',(1.,0.,0.));
#11324=DIRECTION('',(0.,0.,1.));
#11325=DIRECTION('center_axis',(0.,0.,1.));
#11326=DIRECTION('ref_axis',(1.,0.,0.));
#11327=DIRECTION('center_axis',(0.,1.,0.));
#11328=DIRECTION('ref_axis',(-1.,0.,0.));
#11329=DIRECTION('',(-1.,0.,0.));
#11330=DIRECTION('',(0.,0.,1.));
#11331=DIRECTION('',(0.,0.,1.));
#11332=DIRECTION('center_axis',(1.,0.,0.));
#11333=DIRECTION('ref_axis',(0.,1.,0.));
#11334=DIRECTION('',(0.,1.,0.));
#11335=DIRECTION('',(0.,0.,1.));
#11336=DIRECTION('center_axis',(0.,-1.,0.));
#11337=DIRECTION('ref_axis',(1.,0.,0.));
#11338=DIRECTION('',(1.,0.,0.));
#11339=DIRECTION('',(0.,0.,1.));
#11340=DIRECTION('center_axis',(-1.,0.,0.));
#11341=DIRECTION('ref_axis',(0.,-1.,0.));
#11342=DIRECTION('',(0.,-1.,0.));
#11343=DIRECTION('center_axis',(0.,0.,1.));
#11344=DIRECTION('ref_axis',(1.,0.,0.));
#11345=DIRECTION('axis',(0.,0.,1.));
#11346=DIRECTION('refdir',(1.,0.,0.));
#11347=DIRECTION('center_axis',(0.,0.,1.));
#11348=DIRECTION('ref_axis',(1.,0.,0.));
#11349=DIRECTION('',(0.,0.,1.));
#11350=DIRECTION('center_axis',(0.,0.,1.));
#11351=DIRECTION('ref_axis',(1.,0.,0.));
#11352=DIRECTION('',(0.,0.,1.));
#11353=DIRECTION('center_axis',(0.,0.,-1.));
#11354=DIRECTION('ref_axis',(1.,0.,0.));
#11355=DIRECTION('center_axis',(0.,0.,1.));
#11356=DIRECTION('ref_axis',(1.,0.,0.));
#11357=DIRECTION('center_axis',(0.,0.,1.));
#11358=DIRECTION('ref_axis',(1.,0.,0.));
#11359=DIRECTION('',(0.,0.,1.));
#11360=DIRECTION('center_axis',(0.,0.,-1.));
#11361=DIRECTION('ref_axis',(1.,0.,0.));
#11362=DIRECTION('',(0.,0.,1.));
#11363=DIRECTION('center_axis',(0.,0.,1.));
#11364=DIRECTION('ref_axis',(1.,0.,0.));
#11365=DIRECTION('center_axis',(0.,0.,1.));
#11366=DIRECTION('ref_axis',(1.,0.,0.));
#11367=DIRECTION('center_axis',(0.,0.,1.));
#11368=DIRECTION('ref_axis',(1.,0.,0.));
#11369=DIRECTION('center_axis',(0.,0.,-1.));
#11370=DIRECTION('ref_axis',(1.,0.,0.));
#11371=DIRECTION('',(0.,0.,1.));
#11372=DIRECTION('center_axis',(0.,0.,1.));
#11373=DIRECTION('ref_axis',(1.,0.,0.));
#11374=DIRECTION('center_axis',(0.,0.,1.));
#11375=DIRECTION('ref_axis',(1.,0.,0.));
#11376=DIRECTION('center_axis',(0.,0.,1.));
#11377=DIRECTION('ref_axis',(1.,0.,0.));
#11378=DIRECTION('center_axis',(0.,0.,1.));
#11379=DIRECTION('ref_axis',(1.,0.,0.));
#11380=DIRECTION('',(0.,-1.,0.));
#11381=DIRECTION('',(0.,-1.,0.));
#11382=DIRECTION('',(1.,0.,0.));
#11383=DIRECTION('',(0.,1.,0.));
#11384=DIRECTION('',(0.,1.,0.));
#11385=DIRECTION('',(-1.,0.,0.));
#11386=DIRECTION('center_axis',(0.,0.,-1.));
#11387=DIRECTION('ref_axis',(1.,0.,0.));
#11388=DIRECTION('center_axis',(0.,0.,-1.));
#11389=DIRECTION('ref_axis',(1.,0.,0.));
#11390=DIRECTION('center_axis',(0.,0.,-1.));
#11391=DIRECTION('ref_axis',(1.,0.,0.));
#11392=DIRECTION('center_axis',(0.,0.,-1.));
#11393=DIRECTION('ref_axis',(1.,0.,0.));
#11394=DIRECTION('center_axis',(0.,0.,1.));
#11395=DIRECTION('ref_axis',(1.,0.,0.));
#11396=DIRECTION('center_axis',(0.,0.,1.));
#11397=DIRECTION('ref_axis',(1.,0.,0.));
#11398=DIRECTION('',(0.,0.,1.));
#11399=DIRECTION('center_axis',(0.,0.,1.));
#11400=DIRECTION('ref_axis',(1.,0.,0.));
#11401=DIRECTION('center_axis',(0.,0.,1.));
#11402=DIRECTION('ref_axis',(1.,0.,0.));
#11403=DIRECTION('',(0.,0.,1.));
#11404=DIRECTION('center_axis',(0.,0.,1.));
#11405=DIRECTION('ref_axis',(1.,0.,0.));
#11406=DIRECTION('center_axis',(0.,0.,1.));
#11407=DIRECTION('ref_axis',(1.,0.,0.));
#11408=DIRECTION('',(0.,0.,1.));
#11409=DIRECTION('center_axis',(0.,0.,1.));
#11410=DIRECTION('ref_axis',(1.,0.,0.));
#11411=DIRECTION('center_axis',(0.,0.,1.));
#11412=DIRECTION('ref_axis',(1.,0.,0.));
#11413=DIRECTION('center_axis',(0.,0.,1.));
#11414=DIRECTION('ref_axis',(1.,0.,0.));
#11415=DIRECTION('',(0.,0.,1.));
#11416=DIRECTION('center_axis',(0.,0.,1.));
#11417=DIRECTION('ref_axis',(1.,0.,0.));
#11418=DIRECTION('center_axis',(0.,0.,1.));
#11419=DIRECTION('ref_axis',(1.,0.,0.));
#11420=DIRECTION('center_axis',(0.,0.,1.));
#11421=DIRECTION('ref_axis',(1.,0.,0.));
#11422=DIRECTION('',(0.,0.,1.));
#11423=DIRECTION('center_axis',(0.,0.,1.));
#11424=DIRECTION('ref_axis',(1.,0.,0.));
#11425=DIRECTION('center_axis',(0.,0.,1.));
#11426=DIRECTION('ref_axis',(1.,0.,0.));
#11427=DIRECTION('center_axis',(0.,0.,1.));
#11428=DIRECTION('ref_axis',(1.,0.,0.));
#11429=DIRECTION('',(0.,0.,1.));
#11430=DIRECTION('center_axis',(0.,0.,1.));
#11431=DIRECTION('ref_axis',(1.,0.,0.));
#11432=DIRECTION('center_axis',(0.,1.,0.));
#11433=DIRECTION('ref_axis',(-1.,0.,0.));
#11434=DIRECTION('',(-1.,0.,0.));
#11435=DIRECTION('',(0.,0.,1.));
#11436=DIRECTION('',(0.,0.,1.));
#11437=DIRECTION('center_axis',(1.,0.,0.));
#11438=DIRECTION('ref_axis',(0.,1.,0.));
#11439=DIRECTION('',(0.,1.,0.));
#11440=DIRECTION('',(0.,0.,1.));
#11441=DIRECTION('center_axis',(0.,-1.,0.));
#11442=DIRECTION('ref_axis',(1.,0.,0.));
#11443=DIRECTION('',(1.,0.,0.));
#11444=DIRECTION('',(0.,0.,1.));
#11445=DIRECTION('center_axis',(-1.,0.,0.));
#11446=DIRECTION('ref_axis',(0.,-1.,0.));
#11447=DIRECTION('',(0.,-1.,0.));
#11448=DIRECTION('center_axis',(0.,0.,1.));
#11449=DIRECTION('ref_axis',(1.,0.,0.));
#11450=DIRECTION('axis',(0.,0.,1.));
#11451=DIRECTION('refdir',(1.,0.,0.));
#11452=DIRECTION('center_axis',(0.,1.,0.));
#11453=DIRECTION('ref_axis',(-1.,0.,0.));
#11454=DIRECTION('',(-1.,0.,0.));
#11455=DIRECTION('',(0.,0.,1.));
#11456=DIRECTION('',(-1.,0.,0.));
#11457=DIRECTION('',(0.,0.,1.));
#11458=DIRECTION('center_axis',(1.,0.,0.));
#11459=DIRECTION('ref_axis',(0.,1.,0.));
#11460=DIRECTION('',(0.,1.,0.));
#11461=DIRECTION('',(0.,1.,0.));
#11462=DIRECTION('',(0.,0.,1.));
#11463=DIRECTION('center_axis',(0.,-1.,0.));
#11464=DIRECTION('ref_axis',(1.,0.,0.));
#11465=DIRECTION('',(1.,0.,0.));
#11466=DIRECTION('',(1.,0.,0.));
#11467=DIRECTION('',(0.,0.,1.));
#11468=DIRECTION('center_axis',(-1.,0.,0.));
#11469=DIRECTION('ref_axis',(0.,-1.,0.));
#11470=DIRECTION('',(0.,-1.,0.));
#11471=DIRECTION('',(0.,-1.,0.));
#11472=DIRECTION('center_axis',(0.,0.,1.));
#11473=DIRECTION('ref_axis',(1.,0.,0.));
#11474=DIRECTION('center_axis',(0.,0.,1.));
#11475=DIRECTION('ref_axis',(1.,0.,0.));
#11476=DIRECTION('axis',(0.,0.,1.));
#11477=DIRECTION('refdir',(1.,0.,0.));
#11478=DIRECTION('center_axis',(0.,1.,0.));
#11479=DIRECTION('ref_axis',(-1.,0.,0.));
#11480=DIRECTION('',(-1.,0.,0.));
#11481=DIRECTION('',(0.,0.,1.));
#11482=DIRECTION('',(-1.,0.,0.));
#11483=DIRECTION('',(0.,0.,1.));
#11484=DIRECTION('center_axis',(1.,0.,0.));
#11485=DIRECTION('ref_axis',(0.,1.,0.));
#11486=DIRECTION('',(0.,1.,0.));
#11487=DIRECTION('',(0.,1.,0.));
#11488=DIRECTION('',(0.,0.,1.));
#11489=DIRECTION('center_axis',(0.,-1.,0.));
#11490=DIRECTION('ref_axis',(1.,0.,0.));
#11491=DIRECTION('',(1.,0.,0.));
#11492=DIRECTION('',(1.,0.,0.));
#11493=DIRECTION('',(0.,0.,1.));
#11494=DIRECTION('center_axis',(-1.,0.,0.));
#11495=DIRECTION('ref_axis',(0.,-1.,0.));
#11496=DIRECTION('',(0.,-1.,0.));
#11497=DIRECTION('',(0.,-1.,0.));
#11498=DIRECTION('center_axis',(0.,0.,1.));
#11499=DIRECTION('ref_axis',(1.,0.,0.));
#11500=DIRECTION('center_axis',(0.,0.,1.));
#11501=DIRECTION('ref_axis',(1.,0.,0.));
#11502=DIRECTION('axis',(0.,0.,1.));
#11503=DIRECTION('refdir',(1.,0.,0.));
#11504=DIRECTION('center_axis',(0.,1.,0.));
#11505=DIRECTION('ref_axis',(0.,0.,1.));
#11506=DIRECTION('center_axis',(0.,-1.,0.));
#11507=DIRECTION('ref_axis',(1.,0.,0.));
#11508=DIRECTION('center_axis',(0.,-1.,0.));
#11509=DIRECTION('ref_axis',(1.,0.,0.));
#11510=DIRECTION('center_axis',(0.,-1.,0.));
#11511=DIRECTION('ref_axis',(1.,0.,0.));
#11512=DIRECTION('',(0.707106781186548,0.707106781186547,8.65956056235493E-17));
#11513=DIRECTION('center_axis',(0.,-1.,0.));
#11514=DIRECTION('ref_axis',(1.,0.,0.));
#11515=DIRECTION('center_axis',(0.,-1.,0.));
#11516=DIRECTION('ref_axis',(1.,0.,0.));
#11517=DIRECTION('',(0.,1.,0.));
#11518=DIRECTION('center_axis',(0.,1.,0.));
#11519=DIRECTION('ref_axis',(1.,0.,0.));
#11520=DIRECTION('center_axis',(0.,-1.,0.));
#11521=DIRECTION('ref_axis',(1.,0.,0.));
#11522=DIRECTION('',(-0.707106781186547,0.707106781186548,-8.65956056235493E-17));
#11523=DIRECTION('center_axis',(0.,-1.,0.));
#11524=DIRECTION('ref_axis',(0.,0.,-1.));
#11525=DIRECTION('center_axis',(0.,-1.,0.));
#11526=DIRECTION('ref_axis',(1.,0.,0.));
#11527=DIRECTION('center_axis',(0.,1.,0.));
#11528=DIRECTION('ref_axis',(1.,0.,0.));
#11529=DIRECTION('center_axis',(0.,1.,0.));
#11530=DIRECTION('ref_axis',(1.,0.,0.));
#11531=DIRECTION('',(-0.447213595499958,0.894427190999916,-5.47678698264203E-17));
#11532=DIRECTION('center_axis',(0.,-1.,0.));
#11533=DIRECTION('ref_axis',(1.,0.,0.));
#11534=DIRECTION('center_axis',(0.,1.,0.));
#11535=DIRECTION('ref_axis',(1.,0.,0.));
#11536=DIRECTION('',(0.,1.,0.));
#11537=DIRECTION('center_axis',(0.,1.,0.));
#11538=DIRECTION('ref_axis',(1.,0.,0.));
#11539=DIRECTION('center_axis',(0.,-1.,0.));
#11540=DIRECTION('ref_axis',(1.,0.,0.));
#11541=DIRECTION('',(-0.707106781186547,0.707106781186548,-8.65956056235493E-17));
#11542=DIRECTION('center_axis',(0.,-1.,0.));
#11543=DIRECTION('ref_axis',(0.,0.,-1.));
#11544=DIRECTION('center_axis',(0.866025403784439,0.,-0.5));
#11545=DIRECTION('ref_axis',(0.5,0.,0.866025403784439));
#11546=DIRECTION('',(-0.5,0.,-0.866025403784439));
#11547=DIRECTION('',(0.,-1.,0.));
#11548=DIRECTION('',(0.5,0.,0.866025403784439));
#11549=DIRECTION('',(0.,-1.,0.));
#11550=DIRECTION('center_axis',(1.20185167898973E-16,0.,-1.));
#11551=DIRECTION('ref_axis',(1.,0.,1.20185167898973E-16));
#11552=DIRECTION('',(-1.,0.,-1.20185167898973E-16));
#11553=DIRECTION('',(0.,-1.,0.));
#11554=DIRECTION('',(1.,0.,1.20185167898973E-16));
#11555=DIRECTION('center_axis',(-0.866025403784439,0.,-0.5));
#11556=DIRECTION('ref_axis',(0.5,0.,-0.866025403784439));
#11557=DIRECTION('',(-0.5,0.,0.866025403784439));
#11558=DIRECTION('',(0.,-1.,0.));
#11559=DIRECTION('',(0.5,0.,-0.866025403784439));
#11560=DIRECTION('center_axis',(-0.866025403784439,0.,0.5));
#11561=DIRECTION('ref_axis',(-0.5,0.,-0.866025403784439));
#11562=DIRECTION('',(0.5,0.,0.866025403784439));
#11563=DIRECTION('',(0.,-1.,0.));
#11564=DIRECTION('',(-0.5,0.,-0.866025403784439));
#11565=DIRECTION('center_axis',(-2.40370335797945E-16,0.,1.));
#11566=DIRECTION('ref_axis',(-1.,0.,-2.40370335797945E-16));
#11567=DIRECTION('',(1.,0.,2.40370335797945E-16));
#11568=DIRECTION('',(0.,-1.,0.));
#11569=DIRECTION('',(-1.,0.,-2.40370335797945E-16));
#11570=DIRECTION('center_axis',(0.866025403784439,0.,0.5));
#11571=DIRECTION('ref_axis',(-0.5,0.,0.866025403784439));
#11572=DIRECTION('',(0.5,0.,-0.866025403784439));
#11573=DIRECTION('',(-0.5,0.,0.866025403784439));
#11574=DIRECTION('center_axis',(0.,1.,0.));
#11575=DIRECTION('ref_axis',(1.,0.,0.));
#11576=DIRECTION('center_axis',(0.,-1.,0.));
#11577=DIRECTION('ref_axis',(0.,0.,-1.));
#11578=DIRECTION('axis',(0.,0.,1.));
#11579=DIRECTION('refdir',(1.,0.,0.));
#11580=DIRECTION('axis',(0.,0.,1.));
#11581=DIRECTION('refdir',(1.,0.,0.));
#11582=DIRECTION('center_axis',(0.,1.,0.));
#11583=DIRECTION('ref_axis',(1.,0.,0.));
#11584=DIRECTION('center_axis',(0.,1.,0.));
#11585=DIRECTION('ref_axis',(1.,0.,0.));
#11586=DIRECTION('',(0.,1.,0.));
#11587=DIRECTION('center_axis',(0.,-1.,0.));
#11588=DIRECTION('ref_axis',(1.,0.,0.));
#11589=DIRECTION('center_axis',(0.,1.,0.));
#11590=DIRECTION('ref_axis',(1.,0.,0.));
#11591=DIRECTION('center_axis',(0.,1.,0.));
#11592=DIRECTION('ref_axis',(1.,0.,0.));
#11593=DIRECTION('',(0.,1.,0.));
#11594=DIRECTION('center_axis',(0.,-1.,0.));
#11595=DIRECTION('ref_axis',(1.,0.,0.));
#11596=DIRECTION('center_axis',(6.12323399573677E-17,0.,1.));
#11597=DIRECTION('ref_axis',(1.,0.,0.));
#11598=DIRECTION('center_axis',(-1.22464679914735E-16,1.,0.));
#11599=DIRECTION('ref_axis',(-1.,-1.22464679914735E-16,0.));
#11600=DIRECTION('center_axis',(0.,1.,0.));
#11601=DIRECTION('ref_axis',(0.,0.,1.));
#11602=DIRECTION('',(1.,0.,0.));
#11603=DIRECTION('',(0.850265146687862,0.,0.526354614616295));
#11604=DIRECTION('center_axis',(0.,1.,0.));
#11605=DIRECTION('ref_axis',(1.,0.,0.));
#11606=DIRECTION('center_axis',(0.,1.,0.));
#11607=DIRECTION('ref_axis',(0.,0.,1.));
#11608=DIRECTION('',(1.,0.,0.));
#11609=DIRECTION('center_axis',(0.,1.,0.));
#11610=DIRECTION('ref_axis',(1.,0.,0.));
#11611=DIRECTION('',(0.850265146687862,0.,-0.526354614616295));
#11612=DIRECTION('center_axis',(0.,-1.,0.));
#11613=DIRECTION('ref_axis',(0.,0.,-1.));
#11614=DIRECTION('',(-1.,0.,0.));
#11615=DIRECTION('center_axis',(0.,-1.,0.));
#11616=DIRECTION('ref_axis',(1.,0.,0.));
#11617=DIRECTION('',(-0.850265146687862,0.,-0.526354614616295));
#11618=DIRECTION('center_axis',(-0.526354614616295,0.,0.850265146687862));
#11619=DIRECTION('ref_axis',(0.850265146687862,0.,0.526354614616295));
#11620=DIRECTION('',(0.,1.,0.));
#11621=DIRECTION('',(0.,-1.,0.));
#11622=DIRECTION('center_axis',(0.,-1.,0.));
#11623=DIRECTION('ref_axis',(0.,0.,-1.));
#11624=DIRECTION('',(-1.,0.,0.));
#11625=DIRECTION('',(-0.850265146687862,0.,0.526354614616295));
#11626=DIRECTION('center_axis',(0.,-1.,0.));
#11627=DIRECTION('ref_axis',(1.,0.,0.));
#11628=DIRECTION('center_axis',(0.526354614616295,0.,0.850265146687862));
#11629=DIRECTION('ref_axis',(0.850265146687862,0.,-0.526354614616295));
#11630=DIRECTION('',(0.,-1.,0.));
#11631=DIRECTION('',(0.,1.,0.));
#11632=DIRECTION('center_axis',(0.,0.,1.));
#11633=DIRECTION('ref_axis',(1.,0.,0.));
#11634=DIRECTION('',(0.,-1.,0.));
#11635=DIRECTION('',(1.,0.,0.));
#11636=DIRECTION('',(0.,1.,0.));
#11637=DIRECTION('',(-1.,0.,0.));
#11638=DIRECTION('center_axis',(0.,0.,-1.));
#11639=DIRECTION('ref_axis',(1.,0.,0.));
#11640=DIRECTION('center_axis',(0.,0.,-1.));
#11641=DIRECTION('ref_axis',(1.,0.,0.));
#11642=DIRECTION('',(0.,-1.,0.));
#11643=DIRECTION('',(-1.,0.,0.));
#11644=DIRECTION('',(0.,1.,0.));
#11645=DIRECTION('',(0.,1.,0.));
#11646=DIRECTION('',(1.,0.,0.));
#11647=DIRECTION('',(0.,-1.,0.));
#11648=DIRECTION('center_axis',(0.,1.,0.));
#11649=DIRECTION('ref_axis',(6.12323399573677E-17,0.,1.));
#11650=DIRECTION('center_axis',(0.,1.,0.));
#11651=DIRECTION('ref_axis',(1.,0.,0.));
#11652=DIRECTION('center_axis',(0.,-1.,0.));
#11653=DIRECTION('ref_axis',(1.,0.,0.));
#11654=DIRECTION('center_axis',(0.,1.,0.));
#11655=DIRECTION('ref_axis',(1.,0.,0.));
#11656=DIRECTION('center_axis',(0.,1.,0.));
#11657=DIRECTION('ref_axis',(1.,0.,0.));
#11658=DIRECTION('center_axis',(0.,1.,0.));
#11659=DIRECTION('ref_axis',(-1.,0.,0.));
#11660=DIRECTION('',(-1.,0.,0.));
#11661=DIRECTION('',(0.,0.,1.));
#11662=DIRECTION('',(-1.,0.,0.));
#11663=DIRECTION('',(0.,0.,1.));
#11664=DIRECTION('center_axis',(1.,0.,0.));
#11665=DIRECTION('ref_axis',(0.,1.,0.));
#11666=DIRECTION('',(0.,1.,0.));
#11667=DIRECTION('',(0.,0.,1.));
#11668=DIRECTION('',(0.,1.,0.));
#11669=DIRECTION('center_axis',(0.,-1.,0.));
#11670=DIRECTION('ref_axis',(1.,0.,0.));
#11671=DIRECTION('',(1.,0.,0.));
#11672=DIRECTION('',(0.,0.,1.));
#11673=DIRECTION('',(1.,0.,0.));
#11674=DIRECTION('center_axis',(-1.,0.,0.));
#11675=DIRECTION('ref_axis',(0.,-1.,0.));
#11676=DIRECTION('',(0.,-1.,0.));
#11677=DIRECTION('',(0.,-1.,0.));
#11678=DIRECTION('center_axis',(0.,0.,1.));
#11679=DIRECTION('ref_axis',(1.,0.,0.));
#11680=DIRECTION('center_axis',(0.,0.,1.));
#11681=DIRECTION('ref_axis',(1.,0.,0.));
#11682=DIRECTION('center_axis',(0.,0.,1.));
#11683=DIRECTION('ref_axis',(1.,0.,0.));
#11684=DIRECTION('',(0.,0.,1.));
#11685=DIRECTION('center_axis',(0.,0.,1.));
#11686=DIRECTION('ref_axis',(1.,0.,0.));
#11687=DIRECTION('center_axis',(0.,0.,1.));
#11688=DIRECTION('ref_axis',(1.,0.,0.));
#11689=DIRECTION('',(0.,0.,1.));
#11690=DIRECTION('center_axis',(0.,1.,0.));
#11691=DIRECTION('ref_axis',(-1.,0.,0.));
#11692=DIRECTION('',(-1.,0.,0.));
#11693=DIRECTION('',(0.,0.,1.));
#11694=DIRECTION('',(0.,0.,1.));
#11695=DIRECTION('center_axis',(1.,0.,0.));
#11696=DIRECTION('ref_axis',(0.,1.,0.));
#11697=DIRECTION('',(0.,1.,0.));
#11698=DIRECTION('',(0.,0.,1.));
#11699=DIRECTION('center_axis',(0.,-1.,0.));
#11700=DIRECTION('ref_axis',(1.,0.,0.));
#11701=DIRECTION('',(1.,0.,0.));
#11702=DIRECTION('',(0.,0.,1.));
#11703=DIRECTION('center_axis',(-1.,0.,0.));
#11704=DIRECTION('ref_axis',(0.,-1.,0.));
#11705=DIRECTION('',(0.,-1.,0.));
#11706=DIRECTION('center_axis',(0.,0.,1.));
#11707=DIRECTION('ref_axis',(1.,0.,0.));
#11708=DIRECTION('axis',(0.,0.,1.));
#11709=DIRECTION('refdir',(1.,0.,0.));
#11710=DIRECTION('center_axis',(0.,-1.,0.));
#11711=DIRECTION('ref_axis',(1.,0.,0.));
#11712=DIRECTION('center_axis',(0.,-1.,0.));
#11713=DIRECTION('ref_axis',(1.,0.,0.));
#11714=DIRECTION('',(0.,1.,0.));
#11715=DIRECTION('center_axis',(0.,-1.,0.));
#11716=DIRECTION('ref_axis',(1.,0.,0.));
#11717=DIRECTION('center_axis',(0.,1.,0.));
#11718=DIRECTION('ref_axis',(0.,0.,1.));
#11719=DIRECTION('center_axis',(0.,-1.,0.));
#11720=DIRECTION('ref_axis',(1.,0.,0.));
#11721=DIRECTION('center_axis',(6.12323399573677E-17,0.,1.));
#11722=DIRECTION('ref_axis',(1.,0.,0.));
#11723=DIRECTION('center_axis',(1.22464679914735E-16,-1.,0.));
#11724=DIRECTION('ref_axis',(-1.,-1.22464679914735E-16,0.));
#11725=DIRECTION('center_axis',(0.,-1.,0.));
#11726=DIRECTION('ref_axis',(1.,0.,0.));
#11727=DIRECTION('center_axis',(0.,-1.,0.));
#11728=DIRECTION('ref_axis',(0.,0.,-1.));
#11729=DIRECTION('center_axis',(-0.866025403784438,0.,-0.5));
#11730=DIRECTION('ref_axis',(-0.5,0.,0.866025403784438));
#11731=DIRECTION('',(-0.866025403784438,0.,-0.5));
#11732=DIRECTION('center_axis',(-0.866025403784438,0.,-0.5));
#11733=DIRECTION('ref_axis',(-0.5,0.,0.866025403784438));
#11734=DIRECTION('',(-0.866025403784438,0.,-0.5));
#11735=DIRECTION('center_axis',(0.,-1.,0.));
#11736=DIRECTION('ref_axis',(1.,0.,0.));
#11737=DIRECTION('center_axis',(0.,-1.,0.));
#11738=DIRECTION('ref_axis',(1.,0.,0.));
#11739=DIRECTION('',(0.,1.,0.));
#11740=DIRECTION('center_axis',(0.,-1.,0.));
#11741=DIRECTION('ref_axis',(1.,0.,0.));
#11742=DIRECTION('center_axis',(0.866025403784439,0.,-0.5));
#11743=DIRECTION('ref_axis',(-0.5,0.,-0.866025403784439));
#11744=DIRECTION('',(0.866025403784439,0.,-0.5));
#11745=DIRECTION('center_axis',(0.866025403784439,0.,-0.5));
#11746=DIRECTION('ref_axis',(-0.5,0.,-0.866025403784439));
#11747=DIRECTION('',(0.866025403784439,0.,-0.5));
#11748=DIRECTION('center_axis',(0.,0.,1.));
#11749=DIRECTION('ref_axis',(1.,0.,0.));
#11750=DIRECTION('',(0.,0.,1.));
#11751=DIRECTION('center_axis',(0.,0.,1.));
#11752=DIRECTION('ref_axis',(1.,0.,0.));
#11753=DIRECTION('',(0.,0.,1.));
#11754=DIRECTION('center_axis',(0.,1.,0.));
#11755=DIRECTION('ref_axis',(0.,0.,1.));
#11756=DIRECTION('center_axis',(0.,-1.,0.));
#11757=DIRECTION('ref_axis',(1.,0.,0.));
#11758=DIRECTION('center_axis',(0.,1.,0.));
#11759=DIRECTION('ref_axis',(0.,0.,1.));
#11760=DIRECTION('center_axis',(0.,-1.,0.));
#11761=DIRECTION('ref_axis',(1.,0.,0.));
#11762=DIRECTION('center_axis',(0.,-1.,0.));
#11763=DIRECTION('ref_axis',(1.,0.,0.));
#11764=DIRECTION('center_axis',(0.,-1.,0.));
#11765=DIRECTION('ref_axis',(1.,0.,0.));
#11766=DIRECTION('',(0.,1.,0.));
#11767=DIRECTION('center_axis',(0.,-1.,0.));
#11768=DIRECTION('ref_axis',(0.,0.,-1.));
#11769=DIRECTION('center_axis',(0.,-1.,0.));
#11770=DIRECTION('ref_axis',(1.,0.,0.));
#11771=DIRECTION('center_axis',(0.,-1.,0.));
#11772=DIRECTION('ref_axis',(1.,0.,0.));
#11773=DIRECTION('',(0.,1.,0.));
#11774=DIRECTION('',(0.,0.,1.));
#11775=DIRECTION('',(1.,0.,0.));
#11776=DIRECTION('',(0.,0.,1.));
#11777=DIRECTION('',(1.,0.,0.));
#11778=DIRECTION('axis',(0.,0.,1.));
#11779=DIRECTION('refdir',(1.,0.,0.));
#11780=DIRECTION('center_axis',(0.,1.,0.));
#11781=DIRECTION('ref_axis',(1.,0.,0.));
#11782=DIRECTION('center_axis',(0.,-1.,0.));
#11783=DIRECTION('ref_axis',(1.,0.,0.));
#11784=DIRECTION('',(0.,-1.,0.));
#11785=DIRECTION('center_axis',(0.,-1.,0.));
#11786=DIRECTION('ref_axis',(1.,0.,0.));
#11787=DIRECTION('center_axis',(0.,1.,0.));
#11788=DIRECTION('ref_axis',(1.,0.,0.));
#11789=DIRECTION('center_axis',(0.,1.,0.));
#11790=DIRECTION('ref_axis',(1.,0.,0.));
#11791=DIRECTION('',(0.,-1.,0.));
#11792=DIRECTION('center_axis',(0.,1.,0.));
#11793=DIRECTION('ref_axis',(1.,0.,0.));
#11794=DIRECTION('center_axis',(0.,1.,0.));
#11795=DIRECTION('ref_axis',(1.,0.,0.));
#11796=DIRECTION('center_axis',(0.,1.,0.));
#11797=DIRECTION('ref_axis',(1.,0.,0.));
#11798=DIRECTION('axis',(0.,0.,1.));
#11799=DIRECTION('refdir',(1.,0.,0.));
#11800=DIRECTION('center_axis',(0.866025403784439,0.,-0.5));
#11801=DIRECTION('ref_axis',(0.5,0.,0.866025403784439));
#11802=DIRECTION('',(-0.5,0.,-0.866025403784439));
#11803=DIRECTION('',(0.,-1.,0.));
#11804=DIRECTION('',(0.5,0.,0.866025403784439));
#11805=DIRECTION('',(0.,-1.,0.));
#11806=DIRECTION('center_axis',(1.60246890531964E-16,0.,-1.));
#11807=DIRECTION('ref_axis',(1.,0.,1.60246890531964E-16));
#11808=DIRECTION('',(-1.,0.,-1.60246890531964E-16));
#11809=DIRECTION('',(0.,-1.,0.));
#11810=DIRECTION('',(1.,0.,1.60246890531964E-16));
#11811=DIRECTION('center_axis',(-0.866025403784439,0.,-0.5));
#11812=DIRECTION('ref_axis',(0.5,0.,-0.866025403784439));
#11813=DIRECTION('',(-0.5,0.,0.866025403784439));
#11814=DIRECTION('',(0.,-1.,0.));
#11815=DIRECTION('',(0.5,0.,-0.866025403784439));
#11816=DIRECTION('center_axis',(-0.866025403784439,0.,0.5));
#11817=DIRECTION('ref_axis',(-0.5,0.,-0.866025403784439));
#11818=DIRECTION('',(0.5,0.,0.866025403784439));
#11819=DIRECTION('',(0.,-1.,0.));
#11820=DIRECTION('',(-0.5,0.,-0.866025403784439));
#11821=DIRECTION('center_axis',(-1.60246890531964E-16,0.,1.));
#11822=DIRECTION('ref_axis',(-1.,0.,-1.60246890531964E-16));
#11823=DIRECTION('',(1.,0.,1.60246890531964E-16));
#11824=DIRECTION('',(0.,-1.,0.));
#11825=DIRECTION('',(-1.,0.,-1.60246890531964E-16));
#11826=DIRECTION('center_axis',(0.866025403784439,0.,0.5));
#11827=DIRECTION('ref_axis',(-0.5,0.,0.866025403784439));
#11828=DIRECTION('',(0.5,0.,-0.866025403784439));
#11829=DIRECTION('',(-0.5,0.,0.866025403784439));
#11830=DIRECTION('center_axis',(0.,1.,0.));
#11831=DIRECTION('ref_axis',(1.,0.,0.));
#11832=DIRECTION('center_axis',(0.,-1.,0.));
#11833=DIRECTION('ref_axis',(0.,0.,-1.));
#11834=DIRECTION('center_axis',(0.,1.,0.));
#11835=DIRECTION('ref_axis',(1.,0.,0.));
#11836=DIRECTION('center_axis',(0.,1.,0.));
#11837=DIRECTION('ref_axis',(1.,0.,0.));
#11838=DIRECTION('center_axis',(0.,1.,0.));
#11839=DIRECTION('ref_axis',(0.,0.,1.));
#11840=DIRECTION('center_axis',(0.,-1.,0.));
#11841=DIRECTION('ref_axis',(1.,0.,0.));
#11842=DIRECTION('center_axis',(0.,-1.,0.));
#11843=DIRECTION('ref_axis',(1.,0.,0.));
#11844=DIRECTION('center_axis',(0.,-1.,0.));
#11845=DIRECTION('ref_axis',(1.,0.,0.));
#11846=DIRECTION('',(0.707106781186548,0.707106781186547,8.65956056235493E-17));
#11847=DIRECTION('center_axis',(0.,-1.,0.));
#11848=DIRECTION('ref_axis',(1.,0.,0.));
#11849=DIRECTION('center_axis',(0.,-1.,0.));
#11850=DIRECTION('ref_axis',(1.,0.,0.));
#11851=DIRECTION('',(0.,1.,0.));
#11852=DIRECTION('center_axis',(0.,1.,0.));
#11853=DIRECTION('ref_axis',(1.,0.,0.));
#11854=DIRECTION('center_axis',(0.,-1.,0.));
#11855=DIRECTION('ref_axis',(1.,0.,0.));
#11856=DIRECTION('',(-0.707106781186548,0.707106781186547,-8.65956056235494E-17));
#11857=DIRECTION('center_axis',(0.,-1.,0.));
#11858=DIRECTION('ref_axis',(0.,0.,-1.));
#11859=DIRECTION('center_axis',(0.,-1.,0.));
#11860=DIRECTION('ref_axis',(1.,0.,0.));
#11861=DIRECTION('center_axis',(0.,1.,0.));
#11862=DIRECTION('ref_axis',(1.,0.,0.));
#11863=DIRECTION('center_axis',(0.,1.,0.));
#11864=DIRECTION('ref_axis',(1.,0.,0.));
#11865=DIRECTION('',(-0.447213595499958,0.894427190999916,-5.47678698264203E-17));
#11866=DIRECTION('center_axis',(0.,-1.,0.));
#11867=DIRECTION('ref_axis',(1.,0.,0.));
#11868=DIRECTION('',(0.,1.,0.));
#11869=DIRECTION('axis',(0.,0.,1.));
#11870=DIRECTION('refdir',(1.,0.,0.));
#11871=DIRECTION('center_axis',(0.,0.,1.));
#11872=DIRECTION('ref_axis',(1.,0.,0.));
#11873=DIRECTION('',(0.,-1.,0.));
#11874=DIRECTION('center_axis',(0.,0.,1.));
#11875=DIRECTION('ref_axis',(1.,0.,0.));
#11876=DIRECTION('center_axis',(0.,0.,1.));
#11877=DIRECTION('ref_axis',(1.,0.,0.));
#11878=DIRECTION('',(0.,0.,1.));
#11879=DIRECTION('center_axis',(0.,0.,1.));
#11880=DIRECTION('ref_axis',(1.,0.,0.));
#11881=DIRECTION('',(0.,0.,-1.));
#11882=DIRECTION('center_axis',(0.,0.,1.));
#11883=DIRECTION('ref_axis',(-1.,1.22464679914735E-16,0.));
#11884=DIRECTION('',(0.,0.,-1.));
#11885=DIRECTION('center_axis',(0.,0.,1.));
#11886=DIRECTION('ref_axis',(1.,0.,0.));
#11887=DIRECTION('',(0.,0.,1.));
#11888=DIRECTION('center_axis',(0.,0.,1.));
#11889=DIRECTION('ref_axis',(1.,0.,0.));
#11890=DIRECTION('center_axis',(0.,0.,1.));
#11891=DIRECTION('ref_axis',(1.,0.,0.));
#11892=DIRECTION('',(0.,1.,0.));
#11893=DIRECTION('center_axis',(0.,0.,1.));
#11894=DIRECTION('ref_axis',(1.,0.,0.));
#11895=DIRECTION('',(0.,1.,0.));
#11896=DIRECTION('',(1.,0.,0.));
#11897=DIRECTION('',(0.,-1.,0.));
#11898=DIRECTION('',(-1.,0.,0.));
#11899=DIRECTION('',(0.,1.,0.));
#11900=DIRECTION('center_axis',(0.,0.,-1.));
#11901=DIRECTION('ref_axis',(1.,0.,0.));
#11902=DIRECTION('center_axis',(-1.,0.,0.));
#11903=DIRECTION('ref_axis',(0.,0.,1.));
#11904=DIRECTION('',(0.,0.,-1.));
#11905=DIRECTION('',(0.,1.,0.));
#11906=DIRECTION('',(0.,0.,1.));
#11907=DIRECTION('center_axis',(1.,0.,0.));
#11908=DIRECTION('ref_axis',(0.,0.,-1.));
#11909=DIRECTION('center_axis',(0.,0.,1.));
#11910=DIRECTION('ref_axis',(1.,0.,0.));
#11911=DIRECTION('',(0.,1.,0.));
#11912=DIRECTION('',(1.,0.,0.));
#11913=DIRECTION('',(0.,1.,0.));
#11914=DIRECTION('',(0.,1.,0.));
#11915=DIRECTION('',(-1.,0.,0.));
#11916=DIRECTION('center_axis',(0.,0.,-1.));
#11917=DIRECTION('ref_axis',(1.,0.,0.));
#11918=DIRECTION('center_axis',(1.,0.,0.));
#11919=DIRECTION('ref_axis',(0.,0.,-1.));
#11920=DIRECTION('center_axis',(1.,0.,0.));
#11921=DIRECTION('ref_axis',(0.,0.,-1.));
#11922=DIRECTION('',(1.,0.,0.));
#11923=DIRECTION('center_axis',(-1.,0.,0.));
#11924=DIRECTION('ref_axis',(0.,0.,-1.));
#11925=DIRECTION('center_axis',(1.,0.,0.));
#11926=DIRECTION('ref_axis',(0.,0.,-1.));
#11927=DIRECTION('',(1.,0.,0.));
#11928=DIRECTION('center_axis',(-1.,0.,0.));
#11929=DIRECTION('ref_axis',(0.,0.,-1.));
#11930=DIRECTION('center_axis',(0.,0.,1.));
#11931=DIRECTION('ref_axis',(1.,0.,0.));
#11932=DIRECTION('center_axis',(0.,0.,1.));
#11933=DIRECTION('ref_axis',(1.,0.,0.));
#11934=DIRECTION('',(0.,0.,1.));
#11935=DIRECTION('center_axis',(0.,0.,1.));
#11936=DIRECTION('ref_axis',(1.,0.,0.));
#11937=DIRECTION('center_axis',(0.,0.,1.));
#11938=DIRECTION('ref_axis',(1.,0.,0.));
#11939=DIRECTION('',(0.,0.,1.));
#11940=DIRECTION('center_axis',(0.,1.,0.));
#11941=DIRECTION('ref_axis',(1.,0.,0.));
#11942=DIRECTION('center_axis',(0.,1.,0.));
#11943=DIRECTION('ref_axis',(1.,0.,0.));
#11944=DIRECTION('',(0.,1.,0.));
#11945=DIRECTION('center_axis',(0.,-1.,0.));
#11946=DIRECTION('ref_axis',(1.,0.,0.));
#11947=DIRECTION('center_axis',(0.,-1.,0.));
#11948=DIRECTION('ref_axis',(0.,0.,-1.));
#11949=DIRECTION('',(0.,0.,-1.));
#11950=DIRECTION('',(1.,0.,0.));
#11951=DIRECTION('',(0.,0.,1.));
#11952=DIRECTION('',(0.,0.,1.));
#11953=DIRECTION('',(-1.,0.,0.));
#11954=DIRECTION('',(0.,0.,-1.));
#11955=DIRECTION('',(-1.,0.,0.));
#11956=DIRECTION('',(0.,0.,1.));
#11957=DIRECTION('',(-1.,0.,0.));
#11958=DIRECTION('center_axis',(-1.,0.,0.));
#11959=DIRECTION('ref_axis',(0.,0.,1.));
#11960=DIRECTION('',(0.,0.,1.));
#11961=DIRECTION('',(0.,1.,0.));
#11962=DIRECTION('center_axis',(0.,0.,-1.));
#11963=DIRECTION('ref_axis',(-1.,0.,0.));
#11964=DIRECTION('',(-1.,0.,0.));
#11965=DIRECTION('',(0.,1.,0.));
#11966=DIRECTION('center_axis',(1.,0.,0.));
#11967=DIRECTION('ref_axis',(0.,0.,-1.));
#11968=DIRECTION('',(0.,0.,-1.));
#11969=DIRECTION('center_axis',(1.,0.,0.));
#11970=DIRECTION('ref_axis',(0.,0.,-1.));
#11971=DIRECTION('',(0.,0.,-1.));
#11972=DIRECTION('',(0.,1.,0.));
#11973=DIRECTION('center_axis',(0.,0.,1.));
#11974=DIRECTION('ref_axis',(1.,0.,0.));
#11975=DIRECTION('',(1.,0.,0.));
#11976=DIRECTION('',(0.,1.,0.));
#11977=DIRECTION('center_axis',(-1.,0.,0.));
#11978=DIRECTION('ref_axis',(0.,0.,1.));
#11979=DIRECTION('',(0.,0.,1.));
#11980=DIRECTION('',(0.,1.,0.));
#11981=DIRECTION('center_axis',(0.,0.,1.));
#11982=DIRECTION('ref_axis',(1.,0.,0.));
#11983=DIRECTION('',(1.,0.,0.));
#11984=DIRECTION('',(0.,1.,0.));
#11985=DIRECTION('center_axis',(1.,0.,0.));
#11986=DIRECTION('ref_axis',(0.,0.,-1.));
#11987=DIRECTION('',(0.,0.,-1.));
#11988=DIRECTION('',(0.,1.,0.));
#11989=DIRECTION('center_axis',(0.,0.,1.));
#11990=DIRECTION('ref_axis',(1.,0.,0.));
#11991=DIRECTION('',(1.,0.,0.));
#11992=DIRECTION('center_axis',(0.,1.,0.));
#11993=DIRECTION('ref_axis',(0.,0.,1.));
#11994=DIRECTION('axis',(0.,0.,1.));
#11995=DIRECTION('refdir',(1.,0.,0.));
#11996=DIRECTION('center_axis',(0.,1.,0.));
#11997=DIRECTION('ref_axis',(1.,0.,0.));
#11998=DIRECTION('center_axis',(0.,1.,0.));
#11999=DIRECTION('ref_axis',(1.,0.,0.));
#12000=DIRECTION('',(0.707106781186548,-0.707106781186547,-8.65956056235494E-17));
#12001=DIRECTION('center_axis',(0.,-1.,0.));
#12002=DIRECTION('ref_axis',(1.,0.,0.));
#12003=DIRECTION('center_axis',(0.,1.,0.));
#12004=DIRECTION('ref_axis',(1.,0.,0.));
#12005=DIRECTION('',(0.,-1.,0.));
#12006=DIRECTION('center_axis',(0.,-1.,0.));
#12007=DIRECTION('ref_axis',(1.,0.,0.));
#12008=DIRECTION('center_axis',(0.,1.,0.));
#12009=DIRECTION('ref_axis',(1.,0.,0.));
#12010=DIRECTION('center_axis',(0.,1.,0.));
#12011=DIRECTION('ref_axis',(1.,0.,0.));
#12012=DIRECTION('center_axis',(0.,1.,0.));
#12013=DIRECTION('ref_axis',(1.,0.,0.));
#12014=DIRECTION('',(0.,-1.,0.));
#12015=DIRECTION('center_axis',(0.,1.,0.));
#12016=DIRECTION('ref_axis',(1.,0.,0.));
#12017=DIRECTION('center_axis',(0.,1.,0.));
#12018=DIRECTION('ref_axis',(1.,0.,0.));
#12019=DIRECTION('axis',(0.,0.,1.));
#12020=DIRECTION('refdir',(1.,0.,0.));
#12021=DIRECTION('center_axis',(0.866025403784439,0.,-0.5));
#12022=DIRECTION('ref_axis',(0.5,0.,0.866025403784439));
#12023=DIRECTION('',(-0.5,0.,-0.866025403784439));
#12024=DIRECTION('',(0.,-1.,0.));
#12025=DIRECTION('',(0.5,0.,0.866025403784439));
#12026=DIRECTION('',(0.,-1.,0.));
#12027=DIRECTION('center_axis',(1.20185167898973E-16,0.,-1.));
#12028=DIRECTION('ref_axis',(1.,0.,1.20185167898973E-16));
#12029=DIRECTION('',(-1.,0.,-1.20185167898973E-16));
#12030=DIRECTION('',(0.,-1.,0.));
#12031=DIRECTION('',(1.,0.,1.20185167898973E-16));
#12032=DIRECTION('center_axis',(-0.866025403784439,0.,-0.5));
#12033=DIRECTION('ref_axis',(0.5,0.,-0.866025403784439));
#12034=DIRECTION('',(-0.5,0.,0.866025403784439));
#12035=DIRECTION('',(0.,-1.,0.));
#12036=DIRECTION('',(0.5,0.,-0.866025403784439));
#12037=DIRECTION('center_axis',(-0.866025403784439,0.,0.5));
#12038=DIRECTION('ref_axis',(-0.5,0.,-0.866025403784439));
#12039=DIRECTION('',(0.5,0.,0.866025403784439));
#12040=DIRECTION('',(0.,-1.,0.));
#12041=DIRECTION('',(-0.5,0.,-0.866025403784439));
#12042=DIRECTION('center_axis',(-2.40370335797945E-16,0.,1.));
#12043=DIRECTION('ref_axis',(-1.,0.,-2.40370335797945E-16));
#12044=DIRECTION('',(1.,0.,2.40370335797945E-16));
#12045=DIRECTION('',(0.,-1.,0.));
#12046=DIRECTION('',(-1.,0.,-2.40370335797945E-16));
#12047=DIRECTION('center_axis',(0.866025403784439,0.,0.5));
#12048=DIRECTION('ref_axis',(-0.5,0.,0.866025403784439));
#12049=DIRECTION('',(0.5,0.,-0.866025403784439));
#12050=DIRECTION('',(-0.5,0.,0.866025403784439));
#12051=DIRECTION('center_axis',(0.,1.,0.));
#12052=DIRECTION('ref_axis',(1.,0.,0.));
#12053=DIRECTION('center_axis',(0.,-1.,0.));
#12054=DIRECTION('ref_axis',(0.,0.,-1.));
#12055=DIRECTION('center_axis',(0.,1.,0.));
#12056=DIRECTION('ref_axis',(1.,0.,0.));
#12057=DIRECTION('center_axis',(0.,1.,0.));
#12058=DIRECTION('ref_axis',(1.,0.,0.));
#12059=DIRECTION('center_axis',(0.,1.,0.));
#12060=DIRECTION('ref_axis',(0.,0.,1.));
#12061=DIRECTION('center_axis',(0.,-1.,0.));
#12062=DIRECTION('ref_axis',(1.,0.,0.));
#12063=DIRECTION('center_axis',(0.,-1.,0.));
#12064=DIRECTION('ref_axis',(1.,0.,0.));
#12065=DIRECTION('center_axis',(0.,-1.,0.));
#12066=DIRECTION('ref_axis',(1.,0.,0.));
#12067=DIRECTION('',(0.707106781186548,0.707106781186547,8.65956056235493E-17));
#12068=DIRECTION('center_axis',(0.,-1.,0.));
#12069=DIRECTION('ref_axis',(1.,0.,0.));
#12070=DIRECTION('center_axis',(0.,-1.,0.));
#12071=DIRECTION('ref_axis',(1.,0.,0.));
#12072=DIRECTION('',(0.,1.,0.));
#12073=DIRECTION('center_axis',(0.,1.,0.));
#12074=DIRECTION('ref_axis',(1.,0.,0.));
#12075=DIRECTION('center_axis',(0.,-1.,0.));
#12076=DIRECTION('ref_axis',(1.,0.,0.));
#12077=DIRECTION('',(-0.707106781186547,0.707106781186548,-8.65956056235493E-17));
#12078=DIRECTION('center_axis',(0.,-1.,0.));
#12079=DIRECTION('ref_axis',(0.,0.,-1.));
#12080=DIRECTION('center_axis',(0.,-1.,0.));
#12081=DIRECTION('ref_axis',(1.,0.,0.));
#12082=DIRECTION('center_axis',(0.,1.,0.));
#12083=DIRECTION('ref_axis',(1.,0.,0.));
#12084=DIRECTION('center_axis',(0.,1.,0.));
#12085=DIRECTION('ref_axis',(1.,0.,0.));
#12086=DIRECTION('',(-0.447213595499958,0.894427190999916,-5.47678698264203E-17));
#12087=DIRECTION('center_axis',(0.,-1.,0.));
#12088=DIRECTION('ref_axis',(1.,0.,0.));
#12089=DIRECTION('',(0.,1.,0.));
#12090=DIRECTION('axis',(0.,0.,1.));
#12091=DIRECTION('refdir',(1.,0.,0.));
#12092=DIRECTION('center_axis',(0.,1.,0.));
#12093=DIRECTION('ref_axis',(0.,0.,1.));
#12094=DIRECTION('center_axis',(0.,-1.,0.));
#12095=DIRECTION('ref_axis',(1.,0.,0.));
#12096=DIRECTION('center_axis',(0.,-1.,0.));
#12097=DIRECTION('ref_axis',(1.,0.,0.));
#12098=DIRECTION('center_axis',(0.,-1.,0.));
#12099=DIRECTION('ref_axis',(1.,0.,0.));
#12100=DIRECTION('',(0.707106781186547,0.707106781186548,8.65956056235493E-17));
#12101=DIRECTION('center_axis',(0.,-1.,0.));
#12102=DIRECTION('ref_axis',(1.,0.,0.));
#12103=DIRECTION('center_axis',(0.,-1.,0.));
#12104=DIRECTION('ref_axis',(1.,0.,0.));
#12105=DIRECTION('',(0.,1.,0.));
#12106=DIRECTION('center_axis',(0.,1.,0.));
#12107=DIRECTION('ref_axis',(1.,0.,0.));
#12108=DIRECTION('center_axis',(0.,-1.,0.));
#12109=DIRECTION('ref_axis',(1.,0.,0.));
#12110=DIRECTION('',(-0.707106781186547,0.707106781186548,-8.65956056235493E-17));
#12111=DIRECTION('center_axis',(0.,-1.,0.));
#12112=DIRECTION('ref_axis',(0.,0.,-1.));
#12113=DIRECTION('center_axis',(0.,-1.,0.));
#12114=DIRECTION('ref_axis',(1.,0.,0.));
#12115=DIRECTION('center_axis',(0.,1.,0.));
#12116=DIRECTION('ref_axis',(1.,0.,0.));
#12117=DIRECTION('center_axis',(0.,1.,0.));
#12118=DIRECTION('ref_axis',(1.,0.,0.));
#12119=DIRECTION('',(-0.447213595499958,0.894427190999916,-5.47678698264203E-17));
#12120=DIRECTION('center_axis',(0.,-1.,0.));
#12121=DIRECTION('ref_axis',(1.,0.,0.));
#12122=DIRECTION('center_axis',(0.,1.,0.));
#12123=DIRECTION('ref_axis',(1.,0.,0.));
#12124=DIRECTION('',(0.,1.,0.));
#12125=DIRECTION('center_axis',(0.,1.,0.));
#12126=DIRECTION('ref_axis',(1.,0.,0.));
#12127=DIRECTION('center_axis',(0.,-1.,0.));
#12128=DIRECTION('ref_axis',(1.,0.,0.));
#12129=DIRECTION('',(-0.707106781186547,0.707106781186548,-8.65956056235493E-17));
#12130=DIRECTION('center_axis',(0.,-1.,0.));
#12131=DIRECTION('ref_axis',(0.,0.,-1.));
#12132=DIRECTION('center_axis',(0.866025403784439,0.,-0.5));
#12133=DIRECTION('ref_axis',(0.5,0.,0.866025403784439));
#12134=DIRECTION('',(-0.5,0.,-0.866025403784439));
#12135=DIRECTION('',(0.,-1.,0.));
#12136=DIRECTION('',(0.5,0.,0.866025403784439));
#12137=DIRECTION('',(0.,-1.,0.));
#12138=DIRECTION('center_axis',(1.60246890531964E-16,0.,-1.));
#12139=DIRECTION('ref_axis',(1.,0.,1.60246890531964E-16));
#12140=DIRECTION('',(-1.,0.,-1.60246890531964E-16));
#12141=DIRECTION('',(0.,-1.,0.));
#12142=DIRECTION('',(1.,0.,1.60246890531964E-16));
#12143=DIRECTION('center_axis',(-0.866025403784439,0.,-0.5));
#12144=DIRECTION('ref_axis',(0.5,0.,-0.866025403784439));
#12145=DIRECTION('',(-0.5,0.,0.866025403784439));
#12146=DIRECTION('',(0.,-1.,0.));
#12147=DIRECTION('',(0.5,0.,-0.866025403784439));
#12148=DIRECTION('center_axis',(-0.866025403784439,0.,0.5));
#12149=DIRECTION('ref_axis',(-0.5,0.,-0.866025403784439));
#12150=DIRECTION('',(0.5,0.,0.866025403784439));
#12151=DIRECTION('',(0.,-1.,0.));
#12152=DIRECTION('',(-0.5,0.,-0.866025403784439));
#12153=DIRECTION('center_axis',(-1.60246890531964E-16,0.,1.));
#12154=DIRECTION('ref_axis',(-1.,0.,-1.60246890531964E-16));
#12155=DIRECTION('',(1.,0.,1.60246890531964E-16));
#12156=DIRECTION('',(0.,-1.,0.));
#12157=DIRECTION('',(-1.,0.,-1.60246890531964E-16));
#12158=DIRECTION('center_axis',(0.866025403784439,0.,0.5));
#12159=DIRECTION('ref_axis',(-0.5,0.,0.866025403784439));
#12160=DIRECTION('',(0.5,0.,-0.866025403784439));
#12161=DIRECTION('',(-0.5,0.,0.866025403784439));
#12162=DIRECTION('center_axis',(0.,1.,0.));
#12163=DIRECTION('ref_axis',(1.,0.,0.));
#12164=DIRECTION('center_axis',(0.,-1.,0.));
#12165=DIRECTION('ref_axis',(0.,0.,-1.));
#12166=DIRECTION('axis',(0.,0.,1.));
#12167=DIRECTION('refdir',(1.,0.,0.));
#12168=DIRECTION('center_axis',(1.,0.,0.));
#12169=DIRECTION('ref_axis',(0.,0.,-1.));
#12170=DIRECTION('center_axis',(-1.,0.,0.));
#12171=DIRECTION('ref_axis',(0.,0.,-1.));
#12172=DIRECTION('center_axis',(1.,0.,0.));
#12173=DIRECTION('ref_axis',(0.,0.,-1.));
#12174=DIRECTION('center_axis',(-1.,0.,0.));
#12175=DIRECTION('ref_axis',(0.,0.,-1.));
#12176=DIRECTION('',(-0.707106781186548,8.65956056235493E-17,-0.707106781186547));
#12177=DIRECTION('center_axis',(1.,0.,0.));
#12178=DIRECTION('ref_axis',(0.,0.,-1.));
#12179=DIRECTION('center_axis',(1.,0.,0.));
#12180=DIRECTION('ref_axis',(0.,0.,-1.));
#12181=DIRECTION('',(-1.,0.,0.));
#12182=DIRECTION('center_axis',(1.,0.,0.));
#12183=DIRECTION('ref_axis',(0.,0.,-1.));
#12184=DIRECTION('axis',(0.,0.,1.));
#12185=DIRECTION('refdir',(1.,0.,0.));
#12186=DIRECTION('axis',(0.,0.,1.));
#12187=DIRECTION('refdir',(1.,0.,0.));
#12188=DIRECTION('center_axis',(-1.,0.,0.));
#12189=DIRECTION('ref_axis',(0.,0.,1.));
#12190=DIRECTION('',(0.,-1.,0.));
#12191=DIRECTION('',(0.,0.,-1.));
#12192=DIRECTION('',(0.,1.,0.));
#12193=DIRECTION('',(0.,0.,-1.));
#12194=DIRECTION('center_axis',(0.,1.,0.));
#12195=DIRECTION('ref_axis',(1.,0.,0.));
#12196=DIRECTION('center_axis',(0.,-1.,0.));
#12197=DIRECTION('ref_axis',(1.,0.,0.));
#12198=DIRECTION('',(-1.,0.,0.));
#12199=DIRECTION('',(0.,0.,1.));
#12200=DIRECTION('center_axis',(1.,0.,0.));
#12201=DIRECTION('ref_axis',(0.,0.,-1.));
#12202=DIRECTION('',(0.,1.,0.));
#12203=DIRECTION('',(0.,1.,0.));
#12204=DIRECTION('',(0.,0.,1.));
#12205=DIRECTION('center_axis',(0.,0.,1.));
#12206=DIRECTION('ref_axis',(1.,0.,0.));
#12207=DIRECTION('',(-1.,0.,0.));
#12208=DIRECTION('center_axis',(0.,1.,0.));
#12209=DIRECTION('ref_axis',(1.,0.,0.));
#12210=DIRECTION('center_axis',(0.,1.,0.));
#12211=DIRECTION('ref_axis',(1.,0.,0.));
#12212=DIRECTION('',(0.,-1.,0.));
#12213=DIRECTION('center_axis',(0.,1.,0.));
#12214=DIRECTION('ref_axis',(1.,0.,0.));
#12215=DIRECTION('center_axis',(0.,1.,0.));
#12216=DIRECTION('ref_axis',(1.,0.,0.));
#12217=DIRECTION('center_axis',(0.,1.,0.));
#12218=DIRECTION('ref_axis',(1.,0.,0.));
#12219=DIRECTION('center_axis',(0.,1.,0.));
#12220=DIRECTION('ref_axis',(1.,0.,0.));
#12221=DIRECTION('axis',(0.,0.,1.));
#12222=DIRECTION('refdir',(1.,0.,0.));
#12223=DIRECTION('center_axis',(0.,0.,1.));
#12224=DIRECTION('ref_axis',(1.,0.,0.));
#12225=DIRECTION('',(0.,1.,0.));
#12226=DIRECTION('center_axis',(0.,0.,1.));
#12227=DIRECTION('ref_axis',(1.,0.,0.));
#12228=DIRECTION('center_axis',(0.,0.,1.));
#12229=DIRECTION('ref_axis',(1.,0.,0.));
#12230=DIRECTION('center_axis',(0.,0.,1.));
#12231=DIRECTION('ref_axis',(1.,0.,0.));
#12232=DIRECTION('',(0.,0.,1.));
#12233=DIRECTION('center_axis',(0.,0.,1.));
#12234=DIRECTION('ref_axis',(1.,0.,0.));
#12235=DIRECTION('center_axis',(0.,0.,1.));
#12236=DIRECTION('ref_axis',(1.,0.,0.));
#12237=DIRECTION('',(0.,-1.,0.));
#12238=DIRECTION('center_axis',(0.,1.,0.));
#12239=DIRECTION('ref_axis',(1.,0.,0.));
#12240=DIRECTION('center_axis',(0.,-1.,0.));
#12241=DIRECTION('ref_axis',(1.,0.,0.));
#12242=DIRECTION('',(0.,-1.,0.));
#12243=DIRECTION('center_axis',(0.,-1.,0.));
#12244=DIRECTION('ref_axis',(1.,0.,0.));
#12245=DIRECTION('center_axis',(0.,1.,0.));
#12246=DIRECTION('ref_axis',(1.,0.,0.));
#12247=DIRECTION('center_axis',(0.,1.,0.));
#12248=DIRECTION('ref_axis',(1.,0.,0.));
#12249=DIRECTION('',(0.,-1.,0.));
#12250=DIRECTION('center_axis',(0.,1.,0.));
#12251=DIRECTION('ref_axis',(1.,0.,0.));
#12252=DIRECTION('center_axis',(0.,1.,0.));
#12253=DIRECTION('ref_axis',(1.,0.,0.));
#12254=DIRECTION('center_axis',(0.,1.,0.));
#12255=DIRECTION('ref_axis',(1.,0.,0.));
#12256=DIRECTION('axis',(0.,0.,1.));
#12257=DIRECTION('refdir',(1.,0.,0.));
#12258=DIRECTION('center_axis',(0.,0.,1.));
#12259=DIRECTION('ref_axis',(1.,0.,0.));
#12260=DIRECTION('',(0.,1.,0.));
#12261=DIRECTION('center_axis',(0.,0.,1.));
#12262=DIRECTION('ref_axis',(1.,0.,0.));
#12263=DIRECTION('center_axis',(0.,0.,1.));
#12264=DIRECTION('ref_axis',(1.,0.,0.));
#12265=DIRECTION('center_axis',(0.,0.,1.));
#12266=DIRECTION('ref_axis',(1.,0.,0.));
#12267=DIRECTION('',(0.,0.,1.));
#12268=DIRECTION('center_axis',(0.,0.,1.));
#12269=DIRECTION('ref_axis',(1.,0.,0.));
#12270=DIRECTION('center_axis',(0.,0.,1.));
#12271=DIRECTION('ref_axis',(1.,0.,0.));
#12272=DIRECTION('',(0.,-1.,0.));
#12273=DIRECTION('center_axis',(0.,1.,0.));
#12274=DIRECTION('ref_axis',(1.,0.,0.));
#12275=DIRECTION('center_axis',(0.,-1.,0.));
#12276=DIRECTION('ref_axis',(1.,0.,0.));
#12277=DIRECTION('',(0.,-1.,0.));
#12278=DIRECTION('center_axis',(0.,-1.,0.));
#12279=DIRECTION('ref_axis',(1.,0.,0.));
#12280=DIRECTION('center_axis',(0.,1.,0.));
#12281=DIRECTION('ref_axis',(1.,0.,0.));
#12282=DIRECTION('center_axis',(0.,1.,0.));
#12283=DIRECTION('ref_axis',(1.,0.,0.));
#12284=DIRECTION('',(0.,-1.,0.));
#12285=DIRECTION('center_axis',(0.,1.,0.));
#12286=DIRECTION('ref_axis',(1.,0.,0.));
#12287=DIRECTION('center_axis',(0.,1.,0.));
#12288=DIRECTION('ref_axis',(1.,0.,0.));
#12289=DIRECTION('center_axis',(0.,1.,0.));
#12290=DIRECTION('ref_axis',(1.,0.,0.));
#12291=DIRECTION('axis',(0.,0.,1.));
#12292=DIRECTION('refdir',(1.,0.,0.));
#12293=DIRECTION('center_axis',(0.,1.,0.));
#12294=DIRECTION('ref_axis',(1.,0.,0.));
#12295=DIRECTION('center_axis',(0.,-1.,0.));
#12296=DIRECTION('ref_axis',(1.,0.,0.));
#12297=DIRECTION('',(0.,-1.,0.));
#12298=DIRECTION('center_axis',(0.,-1.,0.));
#12299=DIRECTION('ref_axis',(1.,0.,0.));
#12300=DIRECTION('center_axis',(0.,1.,0.));
#12301=DIRECTION('ref_axis',(1.,0.,0.));
#12302=DIRECTION('center_axis',(0.,1.,0.));
#12303=DIRECTION('ref_axis',(1.,0.,0.));
#12304=DIRECTION('',(0.,-1.,0.));
#12305=DIRECTION('center_axis',(0.,1.,0.));
#12306=DIRECTION('ref_axis',(1.,0.,0.));
#12307=DIRECTION('center_axis',(0.,1.,0.));
#12308=DIRECTION('ref_axis',(1.,0.,0.));
#12309=DIRECTION('center_axis',(0.,1.,0.));
#12310=DIRECTION('ref_axis',(1.,0.,0.));
#12311=DIRECTION('axis',(0.,0.,1.));
#12312=DIRECTION('refdir',(1.,0.,0.));
#12313=DIRECTION('center_axis',(0.,1.,0.));
#12314=DIRECTION('ref_axis',(-1.,0.,1.22464679914735E-16));
#12315=DIRECTION('',(0.,1.,0.));
#12316=DIRECTION('center_axis',(0.,1.,0.));
#12317=DIRECTION('ref_axis',(1.,0.,0.));
#12318=DIRECTION('',(0.,-1.,0.));
#12319=DIRECTION('center_axis',(0.,-1.,0.));
#12320=DIRECTION('ref_axis',(1.,0.,0.));
#12321=DIRECTION('center_axis',(0.,1.,0.));
#12322=DIRECTION('ref_axis',(1.,0.,0.));
#12323=DIRECTION('center_axis',(0.,1.,0.));
#12324=DIRECTION('ref_axis',(1.,0.,0.));
#12325=DIRECTION('',(0.,0.,-1.));
#12326=DIRECTION('',(1.,0.,0.));
#12327=DIRECTION('',(0.,0.,1.));
#12328=DIRECTION('center_axis',(0.,-1.,0.));
#12329=DIRECTION('ref_axis',(1.,0.,0.));
#12330=DIRECTION('center_axis',(0.,1.,0.));
#12331=DIRECTION('ref_axis',(1.,0.,0.));
#12332=DIRECTION('center_axis',(0.,1.,0.));
#12333=DIRECTION('ref_axis',(1.,0.,0.));
#12334=DIRECTION('',(0.,1.,0.));
#12335=DIRECTION('center_axis',(0.,-1.,0.));
#12336=DIRECTION('ref_axis',(1.,0.,0.));
#12337=DIRECTION('center_axis',(0.,1.,0.));
#12338=DIRECTION('ref_axis',(1.,0.,0.));
#12339=DIRECTION('center_axis',(0.,0.,1.));
#12340=DIRECTION('ref_axis',(1.,0.,0.));
#12341=DIRECTION('',(0.,-1.,0.));
#12342=DIRECTION('center_axis',(0.,0.,1.));
#12343=DIRECTION('ref_axis',(1.,0.,0.));
#12344=DIRECTION('center_axis',(0.,0.,1.));
#12345=DIRECTION('ref_axis',(5.0532154980743E-16,1.,0.));
#12346=DIRECTION('center_axis',(0.,0.,1.));
#12347=DIRECTION('ref_axis',(1.,0.,0.));
#12348=DIRECTION('',(0.,0.,-1.));
#12349=DIRECTION('',(0.,0.,1.));
#12350=DIRECTION('center_axis',(0.,0.,1.));
#12351=DIRECTION('ref_axis',(1.,0.,0.));
#12352=DIRECTION('',(0.,1.,0.));
#12353=DIRECTION('center_axis',(0.,1.,0.));
#12354=DIRECTION('ref_axis',(6.12323399573677E-17,0.,1.));
#12355=DIRECTION('center_axis',(0.,-1.,0.));
#12356=DIRECTION('ref_axis',(1.,0.,0.));
#12357=DIRECTION('',(0.,1.,0.));
#12358=DIRECTION('',(0.,-1.,0.));
#12359=DIRECTION('center_axis',(0.,-1.,0.));
#12360=DIRECTION('ref_axis',(1.,0.,0.));
#12361=DIRECTION('center_axis',(-1.,0.,0.));
#12362=DIRECTION('ref_axis',(0.,0.,1.));
#12363=DIRECTION('',(0.,0.,1.));
#12364=DIRECTION('',(0.,1.,0.));
#12365=DIRECTION('center_axis',(0.,0.,-1.));
#12366=DIRECTION('ref_axis',(-1.,0.,0.));
#12367=DIRECTION('',(-1.,0.,0.));
#12368=DIRECTION('',(0.,1.,0.));
#12369=DIRECTION('center_axis',(1.,0.,0.));
#12370=DIRECTION('ref_axis',(0.,0.,-1.));
#12371=DIRECTION('',(0.,0.,-1.));
#12372=DIRECTION('center_axis',(0.,1.,0.));
#12373=DIRECTION('ref_axis',(1.,0.,0.));
#12374=DIRECTION('center_axis',(0.,1.,0.));
#12375=DIRECTION('ref_axis',(1.,0.,0.));
#12376=DIRECTION('center_axis',(0.,1.,0.));
#12377=DIRECTION('ref_axis',(1.,0.,0.));
#12378=DIRECTION('center_axis',(0.,1.,0.));
#12379=DIRECTION('ref_axis',(1.,0.,0.));
#12380=DIRECTION('center_axis',(0.,1.,0.));
#12381=DIRECTION('ref_axis',(1.,0.,0.));
#12382=DIRECTION('center_axis',(0.,-1.,0.));
#12383=DIRECTION('ref_axis',(1.,0.,0.));
#12384=DIRECTION('center_axis',(0.,1.,0.));
#12385=DIRECTION('ref_axis',(1.,0.,0.));
#12386=DIRECTION('',(0.,-1.,0.));
#12387=DIRECTION('center_axis',(0.,1.,0.));
#12388=DIRECTION('ref_axis',(1.,0.,0.));
#12389=DIRECTION('',(0.,-1.,0.));
#12390=DIRECTION('center_axis',(0.,1.,0.));
#12391=DIRECTION('ref_axis',(1.,0.,0.));
#12392=DIRECTION('center_axis',(0.,1.,0.));
#12393=DIRECTION('ref_axis',(1.,0.,0.));
#12394=DIRECTION('center_axis',(0.,1.,0.));
#12395=DIRECTION('ref_axis',(-1.,0.,1.22464679914735E-16));
#12396=DIRECTION('center_axis',(0.,1.,0.));
#12397=DIRECTION('ref_axis',(1.,0.,0.));
#12398=DIRECTION('axis',(0.,0.,1.));
#12399=DIRECTION('refdir',(1.,0.,0.));
#12400=DIRECTION('center_axis',(0.,1.,0.));
#12401=DIRECTION('ref_axis',(1.,0.,0.));
#12402=DIRECTION('center_axis',(0.,1.,0.));
#12403=DIRECTION('ref_axis',(1.,0.,0.));
#12404=DIRECTION('',(0.,1.,0.));
#12405=DIRECTION('center_axis',(0.,-1.,0.));
#12406=DIRECTION('ref_axis',(1.,0.,0.));
#12407=DIRECTION('center_axis',(0.,1.,0.));
#12408=DIRECTION('ref_axis',(1.,0.,0.));
#12409=DIRECTION('center_axis',(0.,1.,0.));
#12410=DIRECTION('ref_axis',(1.,0.,0.));
#12411=DIRECTION('center_axis',(0.,1.,0.));
#12412=DIRECTION('ref_axis',(1.,0.,0.));
#12413=DIRECTION('center_axis',(0.,1.,0.));
#12414=DIRECTION('ref_axis',(1.,0.,0.));
#12415=DIRECTION('center_axis',(0.,1.,0.));
#12416=DIRECTION('ref_axis',(1.,0.,0.));
#12417=DIRECTION('center_axis',(0.,1.,0.));
#12418=DIRECTION('ref_axis',(1.,0.,0.));
#12419=DIRECTION('',(0.,-1.,0.));
#12420=DIRECTION('center_axis',(0.,1.,0.));
#12421=DIRECTION('ref_axis',(1.,0.,0.));
#12422=DIRECTION('center_axis',(0.,1.,0.));
#12423=DIRECTION('ref_axis',(1.,0.,0.));
#12424=DIRECTION('',(0.,-1.,0.));
#12425=DIRECTION('center_axis',(0.,1.,0.));
#12426=DIRECTION('ref_axis',(1.,0.,0.));
#12427=DIRECTION('center_axis',(0.,1.,0.));
#12428=DIRECTION('ref_axis',(1.,0.,0.));
#12429=DIRECTION('axis',(0.,0.,1.));
#12430=DIRECTION('refdir',(1.,0.,0.));
#12431=DIRECTION('center_axis',(0.,1.,0.));
#12432=DIRECTION('ref_axis',(1.,0.,0.));
#12433=DIRECTION('center_axis',(0.,-1.,0.));
#12434=DIRECTION('ref_axis',(1.,0.,0.));
#12435=DIRECTION('',(0.,-1.,0.));
#12436=DIRECTION('center_axis',(0.,-1.,0.));
#12437=DIRECTION('ref_axis',(1.,0.,0.));
#12438=DIRECTION('center_axis',(0.,1.,0.));
#12439=DIRECTION('ref_axis',(1.,0.,0.));
#12440=DIRECTION('center_axis',(0.,1.,0.));
#12441=DIRECTION('ref_axis',(1.,0.,0.));
#12442=DIRECTION('',(0.,-1.,0.));
#12443=DIRECTION('center_axis',(0.,1.,0.));
#12444=DIRECTION('ref_axis',(1.,0.,0.));
#12445=DIRECTION('center_axis',(0.,1.,0.));
#12446=DIRECTION('ref_axis',(1.,0.,0.));
#12447=DIRECTION('center_axis',(0.,1.,0.));
#12448=DIRECTION('ref_axis',(1.,0.,0.));
#12449=DIRECTION('axis',(0.,0.,1.));
#12450=DIRECTION('refdir',(1.,0.,0.));
#12451=DIRECTION('center_axis',(0.,1.,0.));
#12452=DIRECTION('ref_axis',(1.,0.,0.));
#12453=DIRECTION('center_axis',(0.,-1.,0.));
#12454=DIRECTION('ref_axis',(1.,0.,0.));
#12455=DIRECTION('',(0.,-1.,0.));
#12456=DIRECTION('center_axis',(0.,-1.,0.));
#12457=DIRECTION('ref_axis',(1.,0.,0.));
#12458=DIRECTION('center_axis',(0.,1.,0.));
#12459=DIRECTION('ref_axis',(1.,0.,0.));
#12460=DIRECTION('center_axis',(0.,1.,0.));
#12461=DIRECTION('ref_axis',(1.,0.,0.));
#12462=DIRECTION('',(0.,-1.,0.));
#12463=DIRECTION('center_axis',(0.,1.,0.));
#12464=DIRECTION('ref_axis',(1.,0.,0.));
#12465=DIRECTION('center_axis',(0.,1.,0.));
#12466=DIRECTION('ref_axis',(1.,0.,0.));
#12467=DIRECTION('center_axis',(0.,1.,0.));
#12468=DIRECTION('ref_axis',(1.,0.,0.));
#12469=DIRECTION('axis',(0.,0.,1.));
#12470=DIRECTION('refdir',(1.,0.,0.));
#12471=DIRECTION('center_axis',(0.,1.,0.));
#12472=DIRECTION('ref_axis',(1.,0.,0.));
#12473=DIRECTION('center_axis',(0.,-1.,0.));
#12474=DIRECTION('ref_axis',(1.,0.,0.));
#12475=DIRECTION('',(0.,-1.,0.));
#12476=DIRECTION('center_axis',(0.,-1.,0.));
#12477=DIRECTION('ref_axis',(1.,0.,0.));
#12478=DIRECTION('center_axis',(0.,1.,0.));
#12479=DIRECTION('ref_axis',(1.,0.,0.));
#12480=DIRECTION('center_axis',(0.,1.,0.));
#12481=DIRECTION('ref_axis',(1.,0.,0.));
#12482=DIRECTION('',(0.,-1.,0.));
#12483=DIRECTION('center_axis',(0.,1.,0.));
#12484=DIRECTION('ref_axis',(1.,0.,0.));
#12485=DIRECTION('center_axis',(0.,1.,0.));
#12486=DIRECTION('ref_axis',(1.,0.,0.));
#12487=DIRECTION('center_axis',(0.,1.,0.));
#12488=DIRECTION('ref_axis',(1.,0.,0.));
#12489=DIRECTION('axis',(0.,0.,1.));
#12490=DIRECTION('refdir',(1.,0.,0.));
#12491=DIRECTION('center_axis',(1.,0.,0.));
#12492=DIRECTION('ref_axis',(0.,0.,-1.));
#12493=DIRECTION('',(0.,-0.707106781186547,-0.707106781186548));
#12494=DIRECTION('',(0.,-1.,0.));
#12495=DIRECTION('',(0.,-0.707106781186547,0.707106781186548));
#12496=DIRECTION('',(0.,0.,1.));
#12497=DIRECTION('',(0.,0.707106781186547,0.707106781186548));
#12498=DIRECTION('',(0.,1.,0.));
#12499=DIRECTION('',(0.,0.707106781186547,-0.707106781186548));
#12500=DIRECTION('',(0.,0.,-1.));
#12501=DIRECTION('center_axis',(0.,0.707106781186548,-0.707106781186547));
#12502=DIRECTION('ref_axis',(-1.,0.,0.));
#12503=DIRECTION('',(1.,0.,0.));
#12504=DIRECTION('',(0.,-0.707106781186547,-0.707106781186548));
#12505=DIRECTION('',(-1.,0.,0.));
#12506=DIRECTION('center_axis',(0.,1.,0.));
#12507=DIRECTION('ref_axis',(-1.,0.,0.));
#12508=DIRECTION('',(-1.,0.,0.));
#12509=DIRECTION('',(0.,0.,-1.));
#12510=DIRECTION('center_axis',(0.,0.707106781186548,0.707106781186547));
#12511=DIRECTION('ref_axis',(1.,0.,0.));
#12512=DIRECTION('',(1.,0.,0.));
#12513=DIRECTION('',(0.,0.707106781186547,-0.707106781186548));
#12514=DIRECTION('center_axis',(0.,0.,1.));
#12515=DIRECTION('ref_axis',(1.,0.,0.));
#12516=DIRECTION('',(-1.,0.,0.));
#12517=DIRECTION('',(0.,1.,0.));
#12518=DIRECTION('center_axis',(1.,0.,0.));
#12519=DIRECTION('ref_axis',(0.,0.,-1.));
#12520=DIRECTION('',(0.,-0.707106781186547,0.707106781186548));
#12521=DIRECTION('',(0.,-1.,0.));
#12522=DIRECTION('',(0.,0.707106781186547,0.707106781186548));
#12523=DIRECTION('',(0.,0.,1.));
#12524=DIRECTION('center_axis',(0.,0.,1.));
#12525=DIRECTION('ref_axis',(1.,0.,0.));
#12526=DIRECTION('',(1.,0.,0.));
#12527=DIRECTION('center_axis',(0.,-0.707106781186548,0.707106781186547));
#12528=DIRECTION('ref_axis',(1.,0.,0.));
#12529=DIRECTION('',(1.,0.,0.));
#12530=DIRECTION('center_axis',(0.,-0.707106781186548,-0.707106781186547));
#12531=DIRECTION('ref_axis',(-1.,0.,0.));
#12532=DIRECTION('',(-1.,0.,0.));
#12533=DIRECTION('center_axis',(0.,-1.,0.));
#12534=DIRECTION('ref_axis',(1.,0.,0.));
#12535=DIRECTION('axis',(0.,0.,1.));
#12536=DIRECTION('refdir',(1.,0.,0.));
#12537=DIRECTION('center_axis',(0.866025403784439,0.,-0.5));
#12538=DIRECTION('ref_axis',(0.5,0.,0.866025403784439));
#12539=DIRECTION('',(0.5,0.,0.866025403784439));
#12540=DIRECTION('',(0.,-1.,0.));
#12541=DIRECTION('',(0.5,0.,0.866025403784439));
#12542=DIRECTION('',(0.,-1.,0.));
#12543=DIRECTION('center_axis',(1.92296268638356E-16,0.,-1.));
#12544=DIRECTION('ref_axis',(1.,0.,1.92296268638356E-16));
#12545=DIRECTION('',(1.,0.,1.92296268638356E-16));
#12546=DIRECTION('',(0.,-1.,0.));
#12547=DIRECTION('',(1.,0.,1.92296268638356E-16));
#12548=DIRECTION('center_axis',(-0.866025403784439,0.,-0.5));
#12549=DIRECTION('ref_axis',(0.5,0.,-0.866025403784439));
#12550=DIRECTION('',(0.5,0.,-0.866025403784439));
#12551=DIRECTION('',(0.,-1.,0.));
#12552=DIRECTION('',(0.5,0.,-0.866025403784438));
#12553=DIRECTION('center_axis',(-0.866025403784439,0.,0.5));
#12554=DIRECTION('ref_axis',(-0.5,0.,-0.866025403784439));
#12555=DIRECTION('',(-0.5,0.,-0.866025403784439));
#12556=DIRECTION('',(0.,-1.,0.));
#12557=DIRECTION('',(-0.5,0.,-0.866025403784439));
#12558=DIRECTION('center_axis',(-1.92296268638356E-16,0.,1.));
#12559=DIRECTION('ref_axis',(-1.,0.,-1.92296268638356E-16));
#12560=DIRECTION('',(-1.,0.,-1.92296268638356E-16));
#12561=DIRECTION('',(0.,-1.,0.));
#12562=DIRECTION('',(-1.,0.,-1.92296268638356E-16));
#12563=DIRECTION('center_axis',(0.866025403784439,0.,0.5));
#12564=DIRECTION('ref_axis',(-0.5,0.,0.866025403784439));
#12565=DIRECTION('',(-0.5,0.,0.866025403784439));
#12566=DIRECTION('',(-0.5,0.,0.866025403784439));
#12567=DIRECTION('center_axis',(0.,-1.,0.));
#12568=DIRECTION('ref_axis',(0.,0.,-1.));
#12569=DIRECTION('center_axis',(0.,1.,0.));
#12570=DIRECTION('ref_axis',(0.,0.,1.));
#12571=DIRECTION('center_axis',(0.,-1.,0.));
#12572=DIRECTION('ref_axis',(1.,0.,0.));
#12573=DIRECTION('center_axis',(0.,-1.,0.));
#12574=DIRECTION('ref_axis',(1.,0.,0.));
#12575=DIRECTION('center_axis',(0.,-1.,0.));
#12576=DIRECTION('ref_axis',(1.,0.,0.));
#12577=DIRECTION('',(0.707106781186547,0.707106781186548,8.65956056235493E-17));
#12578=DIRECTION('center_axis',(0.,-1.,0.));
#12579=DIRECTION('ref_axis',(1.,0.,0.));
#12580=DIRECTION('center_axis',(0.,1.,0.));
#12581=DIRECTION('ref_axis',(1.,0.,0.));
#12582=DIRECTION('',(0.,1.,0.));
#12583=DIRECTION('center_axis',(0.,1.,0.));
#12584=DIRECTION('ref_axis',(1.,0.,0.));
#12585=DIRECTION('center_axis',(0.,-1.,0.));
#12586=DIRECTION('ref_axis',(1.,0.,0.));
#12587=DIRECTION('',(-0.707106781186547,0.707106781186548,-8.65956056235493E-17));
#12588=DIRECTION('center_axis',(0.,-1.,0.));
#12589=DIRECTION('ref_axis',(0.,0.,-1.));
#12590=DIRECTION('axis',(0.,0.,1.));
#12591=DIRECTION('refdir',(1.,0.,0.));
#12592=DIRECTION('axis',(0.,0.,1.));
#12593=DIRECTION('refdir',(1.,0.,0.));
#12594=DIRECTION('center_axis',(0.,1.,0.));
#12595=DIRECTION('ref_axis',(1.,0.,0.));
#12596=DIRECTION('center_axis',(0.,1.,0.));
#12597=DIRECTION('ref_axis',(1.,0.,0.));
#12598=DIRECTION('',(0.,1.,0.));
#12599=DIRECTION('center_axis',(0.,-1.,0.));
#12600=DIRECTION('ref_axis',(1.,0.,0.));
#12601=DIRECTION('center_axis',(0.,1.,0.));
#12602=DIRECTION('ref_axis',(1.,0.,0.));
#12603=DIRECTION('center_axis',(0.,1.,0.));
#12604=DIRECTION('ref_axis',(1.,0.,0.));
#12605=DIRECTION('',(0.,1.,0.));
#12606=DIRECTION('center_axis',(0.,-1.,0.));
#12607=DIRECTION('ref_axis',(1.,0.,0.));
#12608=DIRECTION('center_axis',(0.,1.,0.));
#12609=DIRECTION('ref_axis',(1.,0.,0.));
#12610=DIRECTION('',(0.,1.,0.));
#12611=DIRECTION('center_axis',(0.,1.,0.));
#12612=DIRECTION('ref_axis',(1.,0.,0.));
#12613=DIRECTION('',(0.,-1.,0.));
#12614=DIRECTION('center_axis',(0.,1.,0.));
#12615=DIRECTION('ref_axis',(1.,0.,0.));
#12616=DIRECTION('center_axis',(0.,1.,0.));
#12617=DIRECTION('ref_axis',(0.,0.,1.));
#12618=DIRECTION('',(-1.,0.,0.));
#12619=DIRECTION('center_axis',(0.,1.,0.));
#12620=DIRECTION('ref_axis',(1.,0.,0.));
#12621=DIRECTION('',(1.,0.,0.));
#12622=DIRECTION('center_axis',(0.,0.,-1.));
#12623=DIRECTION('ref_axis',(-1.,0.,0.));
#12624=DIRECTION('',(1.,0.,0.));
#12625=DIRECTION('',(0.,1.,0.));
#12626=DIRECTION('center_axis',(0.,1.,0.));
#12627=DIRECTION('ref_axis',(-1.,0.,1.22464679914735E-16));
#12628=DIRECTION('',(0.,-1.,0.));
#12629=DIRECTION('center_axis',(0.,1.,0.));
#12630=DIRECTION('ref_axis',(1.,0.,0.));
#12631=DIRECTION('center_axis',(0.,0.,1.));
#12632=DIRECTION('ref_axis',(1.,0.,0.));
#12633=DIRECTION('',(-1.,0.,0.));
#12634=DIRECTION('center_axis',(0.,1.,0.));
#12635=DIRECTION('ref_axis',(1.,0.,0.));
#12636=DIRECTION('axis',(0.,0.,1.));
#12637=DIRECTION('refdir',(1.,0.,0.));
#12638=DIRECTION('center_axis',(0.,1.,0.));
#12639=DIRECTION('ref_axis',(1.,0.,0.));
#12640=DIRECTION('center_axis',(0.,-1.,0.));
#12641=DIRECTION('ref_axis',(1.,0.,0.));
#12642=DIRECTION('',(0.,-1.,0.));
#12643=DIRECTION('center_axis',(0.,-1.,0.));
#12644=DIRECTION('ref_axis',(1.,0.,0.));
#12645=DIRECTION('center_axis',(0.,1.,0.));
#12646=DIRECTION('ref_axis',(1.,0.,0.));
#12647=DIRECTION('center_axis',(0.,1.,0.));
#12648=DIRECTION('ref_axis',(1.,0.,0.));
#12649=DIRECTION('',(0.,-1.,0.));
#12650=DIRECTION('center_axis',(0.,1.,0.));
#12651=DIRECTION('ref_axis',(1.,0.,0.));
#12652=DIRECTION('center_axis',(0.,1.,0.));
#12653=DIRECTION('ref_axis',(1.,0.,0.));
#12654=DIRECTION('center_axis',(0.,1.,0.));
#12655=DIRECTION('ref_axis',(1.,0.,0.));
#12656=DIRECTION('axis',(0.,0.,1.));
#12657=DIRECTION('refdir',(1.,0.,0.));
#12658=DIRECTION('center_axis',(0.,1.,0.));
#12659=DIRECTION('ref_axis',(1.,0.,0.));
#12660=DIRECTION('center_axis',(0.,-1.,0.));
#12661=DIRECTION('ref_axis',(1.,0.,0.));
#12662=DIRECTION('',(0.,-1.,0.));
#12663=DIRECTION('center_axis',(0.,-1.,0.));
#12664=DIRECTION('ref_axis',(1.,0.,0.));
#12665=DIRECTION('center_axis',(0.,1.,0.));
#12666=DIRECTION('ref_axis',(1.,0.,0.));
#12667=DIRECTION('center_axis',(0.,1.,0.));
#12668=DIRECTION('ref_axis',(1.,0.,0.));
#12669=DIRECTION('',(0.,-1.,0.));
#12670=DIRECTION('center_axis',(0.,1.,0.));
#12671=DIRECTION('ref_axis',(1.,0.,0.));
#12672=DIRECTION('center_axis',(0.,1.,0.));
#12673=DIRECTION('ref_axis',(1.,0.,0.));
#12674=DIRECTION('center_axis',(0.,1.,0.));
#12675=DIRECTION('ref_axis',(1.,0.,0.));
#12676=DIRECTION('axis',(0.,0.,1.));
#12677=DIRECTION('refdir',(1.,0.,0.));
#12678=DIRECTION('center_axis',(0.,1.,0.));
#12679=DIRECTION('ref_axis',(1.,0.,0.));
#12680=DIRECTION('center_axis',(0.,-1.,0.));
#12681=DIRECTION('ref_axis',(1.,0.,0.));
#12682=DIRECTION('',(0.,-1.,0.));
#12683=DIRECTION('center_axis',(0.,-1.,0.));
#12684=DIRECTION('ref_axis',(1.,0.,0.));
#12685=DIRECTION('center_axis',(0.,1.,0.));
#12686=DIRECTION('ref_axis',(1.,0.,0.));
#12687=DIRECTION('center_axis',(0.,1.,0.));
#12688=DIRECTION('ref_axis',(1.,0.,0.));
#12689=DIRECTION('',(0.,-1.,0.));
#12690=DIRECTION('center_axis',(0.,1.,0.));
#12691=DIRECTION('ref_axis',(1.,0.,0.));
#12692=DIRECTION('center_axis',(0.,1.,0.));
#12693=DIRECTION('ref_axis',(1.,0.,0.));
#12694=DIRECTION('center_axis',(0.,1.,0.));
#12695=DIRECTION('ref_axis',(1.,0.,0.));
#12696=DIRECTION('axis',(0.,0.,1.));
#12697=DIRECTION('refdir',(1.,0.,0.));
#12698=DIRECTION('center_axis',(0.,1.,0.));
#12699=DIRECTION('ref_axis',(1.,0.,0.));
#12700=DIRECTION('center_axis',(0.,-1.,0.));
#12701=DIRECTION('ref_axis',(1.,0.,0.));
#12702=DIRECTION('',(0.,-1.,0.));
#12703=DIRECTION('center_axis',(0.,-1.,0.));
#12704=DIRECTION('ref_axis',(1.,0.,0.));
#12705=DIRECTION('center_axis',(0.,1.,0.));
#12706=DIRECTION('ref_axis',(1.,0.,0.));
#12707=DIRECTION('center_axis',(0.,1.,0.));
#12708=DIRECTION('ref_axis',(1.,0.,0.));
#12709=DIRECTION('',(0.,-1.,0.));
#12710=DIRECTION('center_axis',(0.,1.,0.));
#12711=DIRECTION('ref_axis',(1.,0.,0.));
#12712=DIRECTION('center_axis',(0.,1.,0.));
#12713=DIRECTION('ref_axis',(1.,0.,0.));
#12714=DIRECTION('center_axis',(0.,1.,0.));
#12715=DIRECTION('ref_axis',(1.,0.,0.));
#12716=DIRECTION('axis',(0.,0.,1.));
#12717=DIRECTION('refdir',(1.,0.,0.));
#12718=DIRECTION('axis',(0.,0.,1.));
#12719=DIRECTION('refdir',(1.,0.,0.));
#12720=DIRECTION('center_axis',(0.,-1.,0.));
#12721=DIRECTION('ref_axis',(0.,0.,-1.));
#12722=DIRECTION('center_axis',(0.,-1.,0.));
#12723=DIRECTION('ref_axis',(1.,0.,0.));
#12724=DIRECTION('center_axis',(0.,-1.,0.));
#12725=DIRECTION('ref_axis',(1.,0.,0.));
#12726=DIRECTION('center_axis',(1.,0.,1.22464679914735E-16));
#12727=DIRECTION('ref_axis',(-1.22464679914735E-16,0.,1.));
#12728=DIRECTION('center_axis',(0.,1.,0.));
#12729=DIRECTION('ref_axis',(1.,0.,0.));
#12730=DIRECTION('center_axis',(0.,1.,0.));
#12731=DIRECTION('ref_axis',(1.,0.,0.));
#12732=DIRECTION('center_axis',(0.,-1.,0.));
#12733=DIRECTION('ref_axis',(1.,0.,0.));
#12734=DIRECTION('',(0.,1.,0.));
#12735=DIRECTION('center_axis',(0.,-1.,0.));
#12736=DIRECTION('ref_axis',(1.,0.,0.));
#12737=DIRECTION('center_axis',(0.,-1.,0.));
#12738=DIRECTION('ref_axis',(1.,0.,0.));
#12739=DIRECTION('center_axis',(0.,-1.,0.));
#12740=DIRECTION('ref_axis',(1.,0.,0.));
#12741=DIRECTION('',(0.,1.,0.));
#12742=DIRECTION('center_axis',(0.,-1.,0.));
#12743=DIRECTION('ref_axis',(1.,0.,0.));
#12744=DIRECTION('center_axis',(0.,1.,0.));
#12745=DIRECTION('ref_axis',(1.,0.,0.));
#12746=DIRECTION('',(-0.707106781186547,0.707106781186548,-8.65956056235493E-17));
#12747=DIRECTION('center_axis',(0.,-1.,0.));
#12748=DIRECTION('ref_axis',(1.,0.,0.));
#12749=DIRECTION('center_axis',(0.,1.,0.));
#12750=DIRECTION('ref_axis',(0.,0.,1.));
#12751=DIRECTION('center_axis',(0.,-1.,0.));
#12752=DIRECTION('ref_axis',(1.,0.,0.));
#12753=DIRECTION('center_axis',(0.,-1.,0.));
#12754=DIRECTION('ref_axis',(1.,0.,0.));
#12755=DIRECTION('',(0.,1.,0.));
#12756=DIRECTION('center_axis',(0.,-1.,0.));
#12757=DIRECTION('ref_axis',(0.,0.,-1.));
#12758=DIRECTION('center_axis',(0.,-1.,0.));
#12759=DIRECTION('ref_axis',(1.,0.,0.));
#12760=DIRECTION('center_axis',(0.,-1.,0.));
#12761=DIRECTION('ref_axis',(1.,0.,0.));
#12762=DIRECTION('',(0.707106781186547,0.707106781186548,8.65956056235493E-17));
#12763=DIRECTION('axis',(0.,0.,1.));
#12764=DIRECTION('refdir',(1.,0.,0.));
#12765=DIRECTION('center_axis',(0.,-1.,0.));
#12766=DIRECTION('ref_axis',(0.,0.,-1.));
#12767=DIRECTION('center_axis',(0.,-1.,0.));
#12768=DIRECTION('ref_axis',(1.,0.,0.));
#12769=DIRECTION('center_axis',(0.,-1.,0.));
#12770=DIRECTION('ref_axis',(1.,0.,0.));
#12771=DIRECTION('center_axis',(1.,0.,1.22464679914735E-16));
#12772=DIRECTION('ref_axis',(-1.22464679914735E-16,0.,1.));
#12773=DIRECTION('center_axis',(0.,1.,0.));
#12774=DIRECTION('ref_axis',(1.,0.,0.));
#12775=DIRECTION('center_axis',(0.,1.,0.));
#12776=DIRECTION('ref_axis',(1.,0.,0.));
#12777=DIRECTION('center_axis',(0.,-1.,0.));
#12778=DIRECTION('ref_axis',(1.,0.,0.));
#12779=DIRECTION('center_axis',(0.,-1.,0.));
#12780=DIRECTION('ref_axis',(1.,0.,0.));
#12781=DIRECTION('',(0.,1.,0.));
#12782=DIRECTION('center_axis',(0.,1.,0.));
#12783=DIRECTION('ref_axis',(0.,0.,1.));
#12784=DIRECTION('center_axis',(0.,-1.,0.));
#12785=DIRECTION('ref_axis',(1.,0.,0.));
#12786=DIRECTION('center_axis',(0.,-1.,0.));
#12787=DIRECTION('ref_axis',(1.,0.,0.));
#12788=DIRECTION('center_axis',(0.,-1.,0.));
#12789=DIRECTION('ref_axis',(1.,0.,0.));
#12790=DIRECTION('center_axis',(0.,-1.,0.));
#12791=DIRECTION('ref_axis',(1.,0.,0.));
#12792=DIRECTION('',(0.707106781186548,0.707106781186547,8.65956056235494E-17));
#12793=DIRECTION('center_axis',(0.,-1.,0.));
#12794=DIRECTION('ref_axis',(1.,0.,0.));
#12795=DIRECTION('center_axis',(0.,-1.,0.));
#12796=DIRECTION('ref_axis',(1.,0.,0.));
#12797=DIRECTION('',(0.,1.,0.));
#12798=DIRECTION('center_axis',(0.,1.,0.));
#12799=DIRECTION('ref_axis',(1.,0.,0.));
#12800=DIRECTION('center_axis',(0.,-1.,0.));
#12801=DIRECTION('ref_axis',(1.,0.,0.));
#12802=DIRECTION('',(-0.707106781186548,0.707106781186547,-8.65956056235494E-17));
#12803=DIRECTION('center_axis',(0.,-1.,0.));
#12804=DIRECTION('ref_axis',(0.,0.,-1.));
#12805=DIRECTION('center_axis',(0.,-1.,0.));
#12806=DIRECTION('ref_axis',(1.,0.,0.));
#12807=DIRECTION('',(0.,1.,0.));
#12808=DIRECTION('axis',(0.,0.,1.));
#12809=DIRECTION('refdir',(1.,0.,0.));
#12810=DIRECTION('center_axis',(0.,0.,1.));
#12811=DIRECTION('ref_axis',(1.,0.,0.));
#12812=DIRECTION('center_axis',(1.22464679914735E-16,-1.,0.));
#12813=DIRECTION('ref_axis',(-1.,-1.22464679914735E-16,0.));
#12814=DIRECTION('center_axis',(0.707106781186548,0.,0.707106781186548));
#12815=DIRECTION('ref_axis',(0.707106781186548,0.,-0.707106781186548));
#12816=DIRECTION('center_axis',(8.65956056235494E-17,-1.,-8.65956056235493E-17));
#12817=DIRECTION('ref_axis',(-0.707106781186547,-1.22464679914735E-16,0.707106781186547));
#12818=DIRECTION('center_axis',(1.,0.,0.));
#12819=DIRECTION('ref_axis',(6.12323399573676E-17,0.,-1.));
#12820=DIRECTION('center_axis',(7.49879891330929E-33,-1.,-1.22464679914735E-16));
#12821=DIRECTION('ref_axis',(-6.12323399573676E-17,-1.22464679914735E-16,
1.));
#12822=DIRECTION('center_axis',(0.707106781186548,0.,-0.707106781186548));
#12823=DIRECTION('ref_axis',(-0.707106781186548,0.,-0.707106781186548));
#12824=DIRECTION('center_axis',(-8.65956056235493E-17,-1.,-8.65956056235494E-17));
#12825=DIRECTION('ref_axis',(0.707106781186547,-1.22464679914735E-16,0.707106781186547));
#12826=DIRECTION('center_axis',(0.,0.,-1.));
#12827=DIRECTION('ref_axis',(-1.,0.,-1.22464679914735E-16));
#12828=DIRECTION('center_axis',(-1.22464679914735E-16,-1.,-1.49975978266186E-32));
#12829=DIRECTION('ref_axis',(1.,-1.22464679914735E-16,1.22464679914735E-16));
#12830=DIRECTION('center_axis',(-0.707106781186547,0.,-0.707106781186548));
#12831=DIRECTION('ref_axis',(-0.707106781186548,0.,0.707106781186547));
#12832=DIRECTION('center_axis',(-8.65956056235493E-17,-1.,8.65956056235493E-17));
#12833=DIRECTION('ref_axis',(0.707106781186548,-1.22464679914735E-16,-0.707106781186547));
#12834=DIRECTION('center_axis',(-1.,0.,0.));
#12835=DIRECTION('ref_axis',(-1.83697019872103E-16,0.,1.));
#12836=DIRECTION('center_axis',(-2.24963967399279E-32,-1.,1.22464679914735E-16));
#12837=DIRECTION('ref_axis',(1.83697019872103E-16,-1.22464679914735E-16,
-1.));
#12838=DIRECTION('center_axis',(-0.707106781186548,0.,0.707106781186548));
#12839=DIRECTION('ref_axis',(0.707106781186547,0.,0.707106781186548));
#12840=DIRECTION('center_axis',(8.65956056235493E-17,-1.,8.65956056235493E-17));
#12841=DIRECTION('ref_axis',(-0.707106781186547,-1.22464679914735E-16,-0.707106781186548));
#12842=DIRECTION('axis',(0.,0.,1.));
#12843=DIRECTION('refdir',(1.,0.,0.));
#12844=DIRECTION('center_axis',(0.,0.,1.));
#12845=DIRECTION('ref_axis',(1.,0.,0.));
#12846=DIRECTION('center_axis',(0.,-1.,0.));
#12847=DIRECTION('ref_axis',(0.,0.,-1.));
#12848=DIRECTION('center_axis',(0.,-1.,0.));
#12849=DIRECTION('ref_axis',(0.,0.,-1.));
#12850=DIRECTION('center_axis',(0.,1.,0.));
#12851=DIRECTION('ref_axis',(1.,0.,0.));
#12852=DIRECTION('center_axis',(0.,1.,0.));
#12853=DIRECTION('ref_axis',(1.,0.,0.));
#12854=DIRECTION('center_axis',(0.,1.,0.));
#12855=DIRECTION('ref_axis',(1.,0.,0.));
#12856=DIRECTION('center_axis',(0.,1.,0.));
#12857=DIRECTION('ref_axis',(1.,0.,0.));
#12858=DIRECTION('',(0.,-1.,0.));
#12859=DIRECTION('center_axis',(0.,-1.,0.));
#12860=DIRECTION('ref_axis',(1.,0.,0.));
#12861=DIRECTION('center_axis',(0.,1.,0.));
#12862=DIRECTION('ref_axis',(1.,0.,0.));
#12863=DIRECTION('center_axis',(0.,1.,0.));
#12864=DIRECTION('ref_axis',(1.,0.,0.));
#12865=DIRECTION('center_axis',(0.,1.,0.));
#12866=DIRECTION('ref_axis',(1.,0.,0.));
#12867=DIRECTION('center_axis',(0.,1.,0.));
#12868=DIRECTION('ref_axis',(1.,0.,0.));
#12869=DIRECTION('center_axis',(0.,1.,0.));
#12870=DIRECTION('ref_axis',(1.,0.,0.));
#12871=DIRECTION('center_axis',(0.,1.,0.));
#12872=DIRECTION('ref_axis',(1.,0.,0.));
#12873=DIRECTION('center_axis',(0.,-1.,0.));
#12874=DIRECTION('ref_axis',(1.,0.,0.));
#12875=DIRECTION('center_axis',(0.,-1.,0.));
#12876=DIRECTION('ref_axis',(0.,0.,-1.));
#12877=DIRECTION('center_axis',(6.12323399573677E-17,0.,1.));
#12878=DIRECTION('ref_axis',(1.,0.,0.));
#12879=DIRECTION('center_axis',(0.,-1.,0.));
#12880=DIRECTION('ref_axis',(0.,0.,-1.));
#12881=DIRECTION('center_axis',(0.,1.,0.));
#12882=DIRECTION('ref_axis',(1.,0.,0.));
#12883=DIRECTION('center_axis',(0.,-1.,0.));
#12884=DIRECTION('ref_axis',(1.,0.,0.));
#12885=DIRECTION('center_axis',(0.,-1.,0.));
#12886=DIRECTION('ref_axis',(0.,0.,-1.));
#12887=DIRECTION('center_axis',(0.,0.,1.));
#12888=DIRECTION('ref_axis',(1.,0.,0.));
#12889=DIRECTION('center_axis',(0.,-1.,0.));
#12890=DIRECTION('ref_axis',(0.,0.,-1.));
#12891=DIRECTION('center_axis',(0.,1.,0.));
#12892=DIRECTION('ref_axis',(1.,0.,0.));
#12893=DIRECTION('center_axis',(0.,-1.,0.));
#12894=DIRECTION('ref_axis',(1.,0.,0.));
#12895=DIRECTION('center_axis',(0.,-1.,0.));
#12896=DIRECTION('ref_axis',(0.,0.,-1.));
#12897=DIRECTION('center_axis',(0.,0.,1.));
#12898=DIRECTION('ref_axis',(1.,0.,0.));
#12899=DIRECTION('center_axis',(0.,-1.,0.));
#12900=DIRECTION('ref_axis',(0.,0.,-1.));
#12901=DIRECTION('center_axis',(0.,1.,0.));
#12902=DIRECTION('ref_axis',(1.,0.,0.));
#12903=DIRECTION('center_axis',(0.,-1.,0.));
#12904=DIRECTION('ref_axis',(1.,0.,0.));
#12905=DIRECTION('center_axis',(0.,-1.,0.));
#12906=DIRECTION('ref_axis',(0.,0.,-1.));
#12907=DIRECTION('center_axis',(0.,0.,1.));
#12908=DIRECTION('ref_axis',(1.,0.,0.));
#12909=DIRECTION('center_axis',(0.,-1.,0.));
#12910=DIRECTION('ref_axis',(0.,0.,-1.));
#12911=DIRECTION('center_axis',(0.,1.,0.));
#12912=DIRECTION('ref_axis',(1.,0.,0.));
#12913=DIRECTION('center_axis',(0.,-1.,0.));
#12914=DIRECTION('ref_axis',(1.,0.,0.));
#12915=DIRECTION('center_axis',(0.,-1.,0.));
#12916=DIRECTION('ref_axis',(0.,0.,-1.));
#12917=DIRECTION('center_axis',(6.12323399573676E-17,0.,1.));
#12918=DIRECTION('ref_axis',(1.,0.,0.));
#12919=DIRECTION('center_axis',(0.,-1.,0.));
#12920=DIRECTION('ref_axis',(0.,0.,-1.));
#12921=DIRECTION('center_axis',(0.,1.,0.));
#12922=DIRECTION('ref_axis',(1.,0.,0.));
#12923=DIRECTION('center_axis',(0.,-1.,0.));
#12924=DIRECTION('ref_axis',(1.,0.,0.));
#12925=DIRECTION('center_axis',(0.,-1.,0.));
#12926=DIRECTION('ref_axis',(0.,0.,-1.));
#12927=DIRECTION('center_axis',(0.,0.,1.));
#12928=DIRECTION('ref_axis',(1.,0.,0.));
#12929=DIRECTION('center_axis',(0.,-1.,0.));
#12930=DIRECTION('ref_axis',(0.,0.,-1.));
#12931=DIRECTION('center_axis',(0.,1.,0.));
#12932=DIRECTION('ref_axis',(1.,0.,0.));
#12933=DIRECTION('center_axis',(0.,1.,0.));
#12934=DIRECTION('ref_axis',(1.,0.,0.));
#12935=DIRECTION('',(0.,1.,0.));
#12936=DIRECTION('center_axis',(0.,-1.,0.));
#12937=DIRECTION('ref_axis',(1.,0.,0.));
#12938=DIRECTION('center_axis',(0.,-1.,0.));
#12939=DIRECTION('ref_axis',(1.,0.,0.));
#12940=DIRECTION('center_axis',(0.,1.,0.));
#12941=DIRECTION('ref_axis',(1.,0.,0.));
#12942=DIRECTION('center_axis',(0.,-1.,0.));
#12943=DIRECTION('ref_axis',(0.,0.,-1.));
#12944=DIRECTION('center_axis',(0.,0.,1.));
#12945=DIRECTION('ref_axis',(1.,0.,0.));
#12946=DIRECTION('center_axis',(0.,-1.,0.));
#12947=DIRECTION('ref_axis',(0.,0.,-1.));
#12948=DIRECTION('center_axis',(0.,-1.,0.));
#12949=DIRECTION('ref_axis',(-1.,0.,0.));
#12950=DIRECTION('center_axis',(0.,1.,0.));
#12951=DIRECTION('ref_axis',(1.,0.,0.));
#12952=DIRECTION('axis',(0.,0.,1.));
#12953=DIRECTION('refdir',(1.,0.,0.));
#12954=DIRECTION('center_axis',(0.,1.,0.));
#12955=DIRECTION('ref_axis',(0.,0.,1.));
#12956=DIRECTION('center_axis',(0.,-1.,0.));
#12957=DIRECTION('ref_axis',(1.,0.,0.));
#12958=DIRECTION('center_axis',(0.,-1.,0.));
#12959=DIRECTION('ref_axis',(1.,0.,0.));
#12960=DIRECTION('center_axis',(0.,-1.,0.));
#12961=DIRECTION('ref_axis',(1.,0.,0.));
#12962=DIRECTION('center_axis',(0.,-1.,0.));
#12963=DIRECTION('ref_axis',(1.,0.,0.));
#12964=DIRECTION('',(0.,1.,0.));
#12965=DIRECTION('center_axis',(0.,-1.,0.));
#12966=DIRECTION('ref_axis',(0.,0.,-1.));
#12967=DIRECTION('center_axis',(0.,-1.,0.));
#12968=DIRECTION('ref_axis',(1.,0.,0.));
#12969=DIRECTION('center_axis',(0.,-1.,0.));
#12970=DIRECTION('ref_axis',(1.,0.,0.));
#12971=DIRECTION('',(0.,1.,0.));
#12972=DIRECTION('center_axis',(0.,1.,0.));
#12973=DIRECTION('ref_axis',(0.,0.,1.));
#12974=DIRECTION('center_axis',(0.,-1.,0.));
#12975=DIRECTION('ref_axis',(1.,0.,0.));
#12976=DIRECTION('center_axis',(0.,-1.,0.));
#12977=DIRECTION('ref_axis',(1.,0.,0.));
#12978=DIRECTION('center_axis',(0.,-1.,0.));
#12979=DIRECTION('ref_axis',(1.,0.,0.));
#12980=DIRECTION('center_axis',(0.,-1.,0.));
#12981=DIRECTION('ref_axis',(1.,0.,0.));
#12982=DIRECTION('',(0.,1.,0.));
#12983=DIRECTION('center_axis',(0.,-1.,0.));
#12984=DIRECTION('ref_axis',(0.,0.,-1.));
#12985=DIRECTION('center_axis',(0.,-1.,0.));
#12986=DIRECTION('ref_axis',(1.,0.,0.));
#12987=DIRECTION('center_axis',(0.,-1.,0.));
#12988=DIRECTION('ref_axis',(1.,0.,0.));
#12989=DIRECTION('',(0.,1.,0.));
#12990=DIRECTION('',(0.,0.,1.));
#12991=DIRECTION('',(1.,0.,0.));
#12992=DIRECTION('',(0.,0.,1.));
#12993=DIRECTION('',(1.,0.,0.));
#12994=DIRECTION('',(0.,0.,1.));
#12995=DIRECTION('',(1.,0.,0.));
#12996=DIRECTION('',(0.,0.,1.));
#12997=DIRECTION('',(1.,0.,0.));
#12998=DIRECTION('',(0.,0.,1.));
#12999=DIRECTION('',(1.,0.,0.));
#13000=DIRECTION('',(0.,0.,1.));
#13001=DIRECTION('',(1.,0.,0.));
#13002=DIRECTION('',(0.,0.,1.));
#13003=DIRECTION('',(1.,0.,0.));
#13004=DIRECTION('',(0.,0.,1.));
#13005=DIRECTION('',(1.,0.,0.));
#13006=DIRECTION('',(0.,0.,1.));
#13007=DIRECTION('',(1.,0.,0.));
#13008=DIRECTION('',(0.,0.,1.));
#13009=DIRECTION('',(1.,0.,0.));
#13010=DIRECTION('',(0.,0.,1.));
#13011=DIRECTION('',(1.,0.,0.));
#13012=DIRECTION('',(0.,0.,1.));
#13013=DIRECTION('',(1.,0.,0.));
#13014=DIRECTION('axis',(0.,0.,1.));
#13015=DIRECTION('refdir',(1.,0.,0.));
#13016=DIRECTION('axis',(0.,0.,1.));
#13017=DIRECTION('refdir',(1.,0.,0.));
#13018=DIRECTION('center_axis',(0.,1.,0.));
#13019=DIRECTION('ref_axis',(1.,0.,0.));
#13020=DIRECTION('center_axis',(0.,1.,0.));
#13021=DIRECTION('ref_axis',(1.,0.,0.));
#13022=DIRECTION('',(0.,1.,0.));
#13023=DIRECTION('center_axis',(0.,-1.,0.));
#13024=DIRECTION('ref_axis',(1.,0.,0.));
#13025=DIRECTION('center_axis',(0.,1.,0.));
#13026=DIRECTION('ref_axis',(1.,0.,0.));
#13027=DIRECTION('',(-1.,0.,0.));
#13028=DIRECTION('',(0.,0.,1.));
#13029=DIRECTION('',(-1.,0.,0.));
#13030=DIRECTION('',(0.,0.,-1.));
#13031=DIRECTION('center_axis',(1.,0.,0.));
#13032=DIRECTION('ref_axis',(0.,0.,-1.));
#13033=DIRECTION('',(0.,-1.,0.));
#13034=DIRECTION('',(0.,0.,-1.));
#13035=DIRECTION('',(0.,1.,0.));
#13036=DIRECTION('center_axis',(-1.,0.,0.));
#13037=DIRECTION('ref_axis',(0.,0.,1.));
#13038=DIRECTION('',(0.,1.,0.));
#13039=DIRECTION('',(0.,1.,0.));
#13040=DIRECTION('',(0.,0.,1.));
#13041=DIRECTION('center_axis',(0.,0.,1.));
#13042=DIRECTION('ref_axis',(1.,0.,0.));
#13043=DIRECTION('',(1.,0.,0.));
#13044=DIRECTION('center_axis',(0.,1.,0.));
#13045=DIRECTION('ref_axis',(0.,0.,1.));
#13046=DIRECTION('',(1.,0.,0.));
#13047=DIRECTION('center_axis',(1.,0.,0.));
#13048=DIRECTION('ref_axis',(0.,0.,-1.));
#13049=DIRECTION('center_axis',(1.,0.,0.));
#13050=DIRECTION('ref_axis',(0.,0.,-1.));
#13051=DIRECTION('',(1.,0.,0.));
#13052=DIRECTION('center_axis',(-1.,0.,0.));
#13053=DIRECTION('ref_axis',(0.,0.,-1.));
#13054=DIRECTION('center_axis',(1.,0.,0.));
#13055=DIRECTION('ref_axis',(0.,0.,-1.));
#13056=DIRECTION('center_axis',(1.,0.,0.));
#13057=DIRECTION('ref_axis',(0.,0.,-1.));
#13058=DIRECTION('',(1.,0.,0.));
#13059=DIRECTION('center_axis',(-1.,0.,0.));
#13060=DIRECTION('ref_axis',(0.,0.,-1.));
#13061=DIRECTION('center_axis',(1.,0.,0.));
#13062=DIRECTION('ref_axis',(0.,0.,-1.));
#13063=DIRECTION('center_axis',(1.,0.,0.));
#13064=DIRECTION('ref_axis',(0.,0.,-1.));
#13065=DIRECTION('',(1.,0.,0.));
#13066=DIRECTION('center_axis',(-1.,0.,0.));
#13067=DIRECTION('ref_axis',(0.,0.,-1.));
#13068=DIRECTION('center_axis',(1.,0.,0.));
#13069=DIRECTION('ref_axis',(0.,0.,-1.));
#13070=DIRECTION('center_axis',(1.,0.,0.));
#13071=DIRECTION('ref_axis',(0.,0.,-1.));
#13072=DIRECTION('',(1.,0.,0.));
#13073=DIRECTION('center_axis',(-1.,0.,0.));
#13074=DIRECTION('ref_axis',(0.,0.,-1.));
#13075=DIRECTION('center_axis',(1.,0.,0.));
#13076=DIRECTION('ref_axis',(0.,0.,-1.));
#13077=DIRECTION('center_axis',(1.,0.,0.));
#13078=DIRECTION('ref_axis',(0.,0.,-1.));
#13079=DIRECTION('',(1.,0.,0.));
#13080=DIRECTION('center_axis',(-1.,0.,0.));
#13081=DIRECTION('ref_axis',(0.,0.,-1.));
#13082=DIRECTION('center_axis',(1.,0.,0.));
#13083=DIRECTION('ref_axis',(0.,0.,-1.));
#13084=DIRECTION('center_axis',(1.,0.,0.));
#13085=DIRECTION('ref_axis',(0.,0.,-1.));
#13086=DIRECTION('',(1.,0.,0.));
#13087=DIRECTION('center_axis',(-1.,0.,0.));
#13088=DIRECTION('ref_axis',(0.,0.,-1.));
#13089=DIRECTION('center_axis',(0.,1.,0.));
#13090=DIRECTION('ref_axis',(-1.,0.,0.));
#13091=DIRECTION('',(-1.,0.,0.));
#13092=DIRECTION('',(0.,0.,1.));
#13093=DIRECTION('',(-1.,0.,0.));
#13094=DIRECTION('',(0.,0.,1.));
#13095=DIRECTION('center_axis',(1.,0.,0.));
#13096=DIRECTION('ref_axis',(0.,1.,0.));
#13097=DIRECTION('',(0.,1.,0.));
#13098=DIRECTION('',(0.,1.,0.));
#13099=DIRECTION('',(0.,0.,1.));
#13100=DIRECTION('center_axis',(0.,-1.,0.));
#13101=DIRECTION('ref_axis',(1.,0.,0.));
#13102=DIRECTION('',(1.,0.,0.));
#13103=DIRECTION('',(1.,0.,0.));
#13104=DIRECTION('',(0.,0.,1.));
#13105=DIRECTION('center_axis',(-1.,0.,0.));
#13106=DIRECTION('ref_axis',(0.,-1.,0.));
#13107=DIRECTION('',(0.,-1.,0.));
#13108=DIRECTION('',(0.,-1.,0.));
#13109=DIRECTION('center_axis',(0.,0.,1.));
#13110=DIRECTION('ref_axis',(1.,0.,0.));
#13111=DIRECTION('center_axis',(0.,0.,1.));
#13112=DIRECTION('ref_axis',(1.,0.,0.));
#13113=DIRECTION('axis',(0.,0.,1.));
#13114=DIRECTION('refdir',(1.,0.,0.));
#13115=DIRECTION('center_axis',(1.,0.,0.));
#13116=DIRECTION('ref_axis',(0.,0.,-1.));
#13117=DIRECTION('center_axis',(1.,0.,0.));
#13118=DIRECTION('ref_axis',(0.,0.,-1.));
#13119=DIRECTION('',(1.,0.,0.));
#13120=DIRECTION('center_axis',(-1.,0.,0.));
#13121=DIRECTION('ref_axis',(0.,0.,-1.));
#13122=DIRECTION('center_axis',(1.,0.,0.));
#13123=DIRECTION('ref_axis',(0.,0.,-1.));
#13124=DIRECTION('center_axis',(1.,0.,0.));
#13125=DIRECTION('ref_axis',(0.,0.,-1.));
#13126=DIRECTION('',(1.,0.,0.));
#13127=DIRECTION('center_axis',(-1.,0.,0.));
#13128=DIRECTION('ref_axis',(0.,0.,-1.));
#13129=DIRECTION('center_axis',(1.,0.,0.));
#13130=DIRECTION('ref_axis',(0.,0.,-1.));
#13131=DIRECTION('center_axis',(1.,0.,0.));
#13132=DIRECTION('ref_axis',(0.,0.,-1.));
#13133=DIRECTION('',(1.,0.,0.));
#13134=DIRECTION('center_axis',(-1.,0.,0.));
#13135=DIRECTION('ref_axis',(0.,0.,-1.));
#13136=DIRECTION('center_axis',(1.,0.,0.));
#13137=DIRECTION('ref_axis',(0.,0.,-1.));
#13138=DIRECTION('center_axis',(1.,0.,0.));
#13139=DIRECTION('ref_axis',(0.,0.,-1.));
#13140=DIRECTION('',(1.,0.,0.));
#13141=DIRECTION('center_axis',(-1.,0.,0.));
#13142=DIRECTION('ref_axis',(0.,0.,-1.));
#13143=DIRECTION('center_axis',(1.,0.,0.));
#13144=DIRECTION('ref_axis',(0.,0.,-1.));
#13145=DIRECTION('center_axis',(1.,0.,0.));
#13146=DIRECTION('ref_axis',(0.,0.,-1.));
#13147=DIRECTION('',(1.,0.,0.));
#13148=DIRECTION('center_axis',(-1.,0.,0.));
#13149=DIRECTION('ref_axis',(0.,0.,-1.));
#13150=DIRECTION('center_axis',(1.,0.,0.));
#13151=DIRECTION('ref_axis',(0.,0.,-1.));
#13152=DIRECTION('center_axis',(1.,0.,0.));
#13153=DIRECTION('ref_axis',(0.,0.,-1.));
#13154=DIRECTION('',(1.,0.,0.));
#13155=DIRECTION('center_axis',(-1.,0.,0.));
#13156=DIRECTION('ref_axis',(0.,0.,-1.));
#13157=DIRECTION('center_axis',(0.,1.,0.));
#13158=DIRECTION('ref_axis',(-1.,0.,0.));
#13159=DIRECTION('',(-1.,0.,0.));
#13160=DIRECTION('',(0.,0.,1.));
#13161=DIRECTION('',(-1.,0.,0.));
#13162=DIRECTION('',(0.,0.,1.));
#13163=DIRECTION('center_axis',(1.,0.,0.));
#13164=DIRECTION('ref_axis',(0.,1.,0.));
#13165=DIRECTION('',(0.,1.,0.));
#13166=DIRECTION('',(0.,1.,0.));
#13167=DIRECTION('',(0.,0.,1.));
#13168=DIRECTION('center_axis',(0.,-1.,0.));
#13169=DIRECTION('ref_axis',(1.,0.,0.));
#13170=DIRECTION('',(1.,0.,0.));
#13171=DIRECTION('',(1.,0.,0.));
#13172=DIRECTION('',(0.,0.,1.));
#13173=DIRECTION('center_axis',(-1.,0.,0.));
#13174=DIRECTION('ref_axis',(0.,-1.,0.));
#13175=DIRECTION('',(0.,-1.,0.));
#13176=DIRECTION('',(0.,-1.,0.));
#13177=DIRECTION('center_axis',(0.,0.,1.));
#13178=DIRECTION('ref_axis',(1.,0.,0.));
#13179=DIRECTION('center_axis',(0.,0.,1.));
#13180=DIRECTION('ref_axis',(1.,0.,0.));
#13181=DIRECTION('axis',(0.,0.,1.));
#13182=DIRECTION('refdir',(1.,0.,0.));
#13183=DIRECTION('center_axis',(1.,0.,0.));
#13184=DIRECTION('ref_axis',(0.,0.,-1.));
#13185=DIRECTION('center_axis',(1.,0.,0.));
#13186=DIRECTION('ref_axis',(0.,0.,-1.));
#13187=DIRECTION('',(1.,0.,0.));
#13188=DIRECTION('center_axis',(-1.,0.,0.));
#13189=DIRECTION('ref_axis',(0.,0.,-1.));
#13190=DIRECTION('center_axis',(1.,0.,0.));
#13191=DIRECTION('ref_axis',(0.,0.,-1.));
#13192=DIRECTION('center_axis',(1.,0.,0.));
#13193=DIRECTION('ref_axis',(0.,0.,-1.));
#13194=DIRECTION('',(1.,0.,0.));
#13195=DIRECTION('center_axis',(-1.,0.,0.));
#13196=DIRECTION('ref_axis',(0.,0.,-1.));
#13197=DIRECTION('center_axis',(1.,0.,0.));
#13198=DIRECTION('ref_axis',(0.,0.,-1.));
#13199=DIRECTION('center_axis',(1.,0.,0.));
#13200=DIRECTION('ref_axis',(0.,0.,-1.));
#13201=DIRECTION('',(1.,0.,0.));
#13202=DIRECTION('center_axis',(-1.,0.,0.));
#13203=DIRECTION('ref_axis',(0.,0.,-1.));
#13204=DIRECTION('center_axis',(1.,0.,0.));
#13205=DIRECTION('ref_axis',(0.,0.,-1.));
#13206=DIRECTION('center_axis',(1.,0.,0.));
#13207=DIRECTION('ref_axis',(0.,0.,-1.));
#13208=DIRECTION('',(1.,0.,0.));
#13209=DIRECTION('center_axis',(-1.,0.,0.));
#13210=DIRECTION('ref_axis',(0.,0.,-1.));
#13211=DIRECTION('center_axis',(1.,0.,0.));
#13212=DIRECTION('ref_axis',(0.,0.,-1.));
#13213=DIRECTION('center_axis',(1.,0.,0.));
#13214=DIRECTION('ref_axis',(0.,0.,-1.));
#13215=DIRECTION('',(1.,0.,0.));
#13216=DIRECTION('center_axis',(-1.,0.,0.));
#13217=DIRECTION('ref_axis',(0.,0.,-1.));
#13218=DIRECTION('center_axis',(1.,0.,0.));
#13219=DIRECTION('ref_axis',(0.,0.,-1.));
#13220=DIRECTION('center_axis',(1.,0.,0.));
#13221=DIRECTION('ref_axis',(0.,0.,-1.));
#13222=DIRECTION('',(1.,0.,0.));
#13223=DIRECTION('center_axis',(-1.,0.,0.));
#13224=DIRECTION('ref_axis',(0.,0.,-1.));
#13225=DIRECTION('center_axis',(0.,1.,0.));
#13226=DIRECTION('ref_axis',(-1.,0.,0.));
#13227=DIRECTION('',(-1.,0.,0.));
#13228=DIRECTION('',(0.,0.,1.));
#13229=DIRECTION('',(-1.,0.,0.));
#13230=DIRECTION('',(0.,0.,1.));
#13231=DIRECTION('center_axis',(1.,0.,0.));
#13232=DIRECTION('ref_axis',(0.,1.,0.));
#13233=DIRECTION('',(0.,1.,0.));
#13234=DIRECTION('',(0.,1.,0.));
#13235=DIRECTION('',(0.,0.,1.));
#13236=DIRECTION('center_axis',(0.,-1.,0.));
#13237=DIRECTION('ref_axis',(1.,0.,0.));
#13238=DIRECTION('',(1.,0.,0.));
#13239=DIRECTION('',(1.,0.,0.));
#13240=DIRECTION('',(0.,0.,1.));
#13241=DIRECTION('center_axis',(-1.,0.,0.));
#13242=DIRECTION('ref_axis',(0.,-1.,0.));
#13243=DIRECTION('',(0.,-1.,0.));
#13244=DIRECTION('',(0.,-1.,0.));
#13245=DIRECTION('center_axis',(0.,0.,1.));
#13246=DIRECTION('ref_axis',(1.,0.,0.));
#13247=DIRECTION('center_axis',(0.,0.,1.));
#13248=DIRECTION('ref_axis',(1.,0.,0.));
#13249=DIRECTION('axis',(0.,0.,1.));
#13250=DIRECTION('refdir',(1.,0.,0.));
#13251=DIRECTION('center_axis',(0.,1.,0.));
#13252=DIRECTION('ref_axis',(1.,0.,0.));
#13253=DIRECTION('center_axis',(0.,1.,0.));
#13254=DIRECTION('ref_axis',(1.,0.,0.));
#13255=DIRECTION('',(0.,1.,0.));
#13256=DIRECTION('center_axis',(0.,-1.,0.));
#13257=DIRECTION('ref_axis',(1.,0.,0.));
#13258=DIRECTION('center_axis',(0.,1.,0.));
#13259=DIRECTION('ref_axis',(1.,0.,0.));
#13260=DIRECTION('center_axis',(0.,1.,0.));
#13261=DIRECTION('ref_axis',(1.,0.,0.));
#13262=DIRECTION('center_axis',(0.,1.,0.));
#13263=DIRECTION('ref_axis',(1.,0.,0.));
#13264=DIRECTION('center_axis',(0.,1.,0.));
#13265=DIRECTION('ref_axis',(1.,0.,0.));
#13266=DIRECTION('center_axis',(0.,1.,0.));
#13267=DIRECTION('ref_axis',(1.,0.,0.));
#13268=DIRECTION('',(0.,-1.,0.));
#13269=DIRECTION('center_axis',(0.,1.,0.));
#13270=DIRECTION('ref_axis',(1.,0.,0.));
#13271=DIRECTION('center_axis',(0.,1.,0.));
#13272=DIRECTION('ref_axis',(1.,0.,0.));
#13273=DIRECTION('center_axis',(0.,1.,0.));
#13274=DIRECTION('ref_axis',(1.,0.,0.));
#13275=DIRECTION('center_axis',(0.,1.,0.));
#13276=DIRECTION('ref_axis',(1.,0.,0.));
#13277=DIRECTION('',(0.,-1.,0.));
#13278=DIRECTION('center_axis',(0.,1.,0.));
#13279=DIRECTION('ref_axis',(1.,0.,0.));
#13280=DIRECTION('axis',(0.,0.,1.));
#13281=DIRECTION('refdir',(1.,0.,0.));
#13282=DIRECTION('center_axis',(0.,1.,0.));
#13283=DIRECTION('ref_axis',(1.,0.,0.));
#13284=DIRECTION('center_axis',(0.,-1.,0.));
#13285=DIRECTION('ref_axis',(1.,0.,0.));
#13286=DIRECTION('',(0.,-1.,0.));
#13287=DIRECTION('center_axis',(0.,-1.,0.));
#13288=DIRECTION('ref_axis',(1.,0.,0.));
#13289=DIRECTION('center_axis',(0.,1.,0.));
#13290=DIRECTION('ref_axis',(1.,0.,0.));
#13291=DIRECTION('center_axis',(0.,1.,0.));
#13292=DIRECTION('ref_axis',(1.,0.,0.));
#13293=DIRECTION('',(0.,-1.,0.));
#13294=DIRECTION('center_axis',(0.,1.,0.));
#13295=DIRECTION('ref_axis',(1.,0.,0.));
#13296=DIRECTION('center_axis',(0.,1.,0.));
#13297=DIRECTION('ref_axis',(1.,0.,0.));
#13298=DIRECTION('center_axis',(0.,1.,0.));
#13299=DIRECTION('ref_axis',(1.,0.,0.));
#13300=DIRECTION('axis',(0.,0.,1.));
#13301=DIRECTION('refdir',(1.,0.,0.));
#13302=DIRECTION('center_axis',(0.,1.,0.));
#13303=DIRECTION('ref_axis',(1.,0.,0.));
#13304=DIRECTION('center_axis',(0.,-1.,0.));
#13305=DIRECTION('ref_axis',(1.,0.,0.));
#13306=DIRECTION('',(0.,-1.,0.));
#13307=DIRECTION('center_axis',(0.,-1.,0.));
#13308=DIRECTION('ref_axis',(1.,0.,0.));
#13309=DIRECTION('center_axis',(0.,1.,0.));
#13310=DIRECTION('ref_axis',(1.,0.,0.));
#13311=DIRECTION('center_axis',(0.,1.,0.));
#13312=DIRECTION('ref_axis',(1.,0.,0.));
#13313=DIRECTION('',(0.,-1.,0.));
#13314=DIRECTION('center_axis',(0.,1.,0.));
#13315=DIRECTION('ref_axis',(1.,0.,0.));
#13316=DIRECTION('center_axis',(0.,1.,0.));
#13317=DIRECTION('ref_axis',(1.,0.,0.));
#13318=DIRECTION('center_axis',(0.,1.,0.));
#13319=DIRECTION('ref_axis',(1.,0.,0.));
#13320=DIRECTION('axis',(0.,0.,1.));
#13321=DIRECTION('refdir',(1.,0.,0.));
#13322=DIRECTION('center_axis',(0.,1.,0.));
#13323=DIRECTION('ref_axis',(1.,0.,0.));
#13324=DIRECTION('center_axis',(0.,-1.,0.));
#13325=DIRECTION('ref_axis',(1.,0.,0.));
#13326=DIRECTION('',(0.,-1.,0.));
#13327=DIRECTION('center_axis',(0.,-1.,0.));
#13328=DIRECTION('ref_axis',(1.,0.,0.));
#13329=DIRECTION('center_axis',(0.,1.,0.));
#13330=DIRECTION('ref_axis',(1.,0.,0.));
#13331=DIRECTION('center_axis',(0.,1.,0.));
#13332=DIRECTION('ref_axis',(1.,0.,0.));
#13333=DIRECTION('',(0.,-1.,0.));
#13334=DIRECTION('center_axis',(0.,1.,0.));
#13335=DIRECTION('ref_axis',(1.,0.,0.));
#13336=DIRECTION('center_axis',(0.,1.,0.));
#13337=DIRECTION('ref_axis',(1.,0.,0.));
#13338=DIRECTION('center_axis',(0.,1.,0.));
#13339=DIRECTION('ref_axis',(1.,0.,0.));
#13340=DIRECTION('axis',(0.,0.,1.));
#13341=DIRECTION('refdir',(1.,0.,0.));
#13342=DIRECTION('axis',(0.,0.,1.));
#13343=DIRECTION('refdir',(1.,0.,0.));
#13344=DIRECTION('center_axis',(0.,1.,0.));
#13345=DIRECTION('ref_axis',(0.,0.,1.));
#13346=DIRECTION('center_axis',(0.,-1.,0.));
#13347=DIRECTION('ref_axis',(1.,0.,0.));
#13348=DIRECTION('',(-1.,0.,0.));
#13349=DIRECTION('',(0.,0.,-1.));
#13350=DIRECTION('',(1.,0.,0.));
#13351=DIRECTION('center_axis',(0.,0.,1.));
#13352=DIRECTION('ref_axis',(1.,0.,0.));
#13353=DIRECTION('',(0.,-1.,0.));
#13354=DIRECTION('',(0.,1.,0.));
#13355=DIRECTION('',(-1.,0.,0.));
#13356=DIRECTION('center_axis',(0.,-1.,0.));
#13357=DIRECTION('ref_axis',(0.,0.,-1.));
#13358=DIRECTION('center_axis',(0.,1.,0.));
#13359=DIRECTION('ref_axis',(1.,0.,0.));
#13360=DIRECTION('',(0.,0.,1.));
#13361=DIRECTION('',(1.,0.,0.));
#13362=DIRECTION('center_axis',(0.,0.,-1.));
#13363=DIRECTION('ref_axis',(-1.,0.,0.));
#13364=DIRECTION('',(0.,1.,0.));
#13365=DIRECTION('',(0.,1.,0.));
#13366=DIRECTION('center_axis',(1.,0.,0.));
#13367=DIRECTION('ref_axis',(0.,0.,-1.));
#13368=DIRECTION('center_axis',(0.,1.,0.));
#13369=DIRECTION('ref_axis',(0.,0.,1.));
#13370=DIRECTION('center_axis',(0.,-1.,0.));
#13371=DIRECTION('ref_axis',(1.,0.,0.));
#13372=DIRECTION('center_axis',(0.,-1.,0.));
#13373=DIRECTION('ref_axis',(1.,0.,0.));
#13374=DIRECTION('center_axis',(0.,-1.,0.));
#13375=DIRECTION('ref_axis',(1.,0.,0.));
#13376=DIRECTION('center_axis',(0.,-1.,0.));
#13377=DIRECTION('ref_axis',(1.,0.,0.));
#13378=DIRECTION('',(0.,1.,0.));
#13379=DIRECTION('center_axis',(0.,-1.,0.));
#13380=DIRECTION('ref_axis',(0.,0.,-1.));
#13381=DIRECTION('center_axis',(0.,-1.,0.));
#13382=DIRECTION('ref_axis',(1.,0.,0.));
#13383=DIRECTION('center_axis',(0.,-1.,0.));
#13384=DIRECTION('ref_axis',(1.,0.,0.));
#13385=DIRECTION('center_axis',(0.,-1.,0.));
#13386=DIRECTION('ref_axis',(1.,0.,0.));
#13387=DIRECTION('',(0.,1.,0.));
#13388=DIRECTION('center_axis',(0.,1.,0.));
#13389=DIRECTION('ref_axis',(0.,0.,1.));
#13390=DIRECTION('center_axis',(0.,-1.,0.));
#13391=DIRECTION('ref_axis',(1.,0.,0.));
#13392=DIRECTION('center_axis',(0.,-1.,0.));
#13393=DIRECTION('ref_axis',(1.,0.,0.));
#13394=DIRECTION('center_axis',(0.,-1.,0.));
#13395=DIRECTION('ref_axis',(1.,0.,0.));
#13396=DIRECTION('',(0.,1.,0.));
#13397=DIRECTION('center_axis',(0.,-1.,0.));
#13398=DIRECTION('ref_axis',(0.,0.,-1.));
#13399=DIRECTION('center_axis',(0.,-1.,0.));
#13400=DIRECTION('ref_axis',(1.,0.,0.));
#13401=DIRECTION('center_axis',(0.,-1.,0.));
#13402=DIRECTION('ref_axis',(1.,0.,0.));
#13403=DIRECTION('center_axis',(0.,-1.,0.));
#13404=DIRECTION('ref_axis',(1.,0.,0.));
#13405=DIRECTION('',(0.,1.,0.));
#13406=DIRECTION('center_axis',(0.,1.,0.));
#13407=DIRECTION('ref_axis',(0.,0.,1.));
#13408=DIRECTION('center_axis',(0.,-1.,0.));
#13409=DIRECTION('ref_axis',(1.,0.,0.));
#13410=DIRECTION('center_axis',(0.,-1.,0.));
#13411=DIRECTION('ref_axis',(1.,0.,0.));
#13412=DIRECTION('center_axis',(0.,-1.,0.));
#13413=DIRECTION('ref_axis',(1.,0.,0.));
#13414=DIRECTION('',(0.,1.,0.));
#13415=DIRECTION('center_axis',(0.,-1.,0.));
#13416=DIRECTION('ref_axis',(0.,0.,-1.));
#13417=DIRECTION('center_axis',(0.,-1.,0.));
#13418=DIRECTION('ref_axis',(1.,0.,0.));
#13419=DIRECTION('center_axis',(0.,-1.,0.));
#13420=DIRECTION('ref_axis',(1.,0.,0.));
#13421=DIRECTION('',(0.,1.,0.));
#13422=DIRECTION('axis',(0.,0.,1.));
#13423=DIRECTION('refdir',(1.,0.,0.));
#13424=DIRECTION('center_axis',(0.,1.,0.));
#13425=DIRECTION('ref_axis',(0.,0.,1.));
#13426=DIRECTION('center_axis',(0.,1.,0.));
#13427=DIRECTION('ref_axis',(1.,0.,0.));
#13428=DIRECTION('',(1.,0.,0.));
#13429=DIRECTION('center_axis',(0.,-1.,0.));
#13430=DIRECTION('ref_axis',(1.,0.,0.));
#13431=DIRECTION('',(-1.,0.,0.));
#13432=DIRECTION('center_axis',(0.,0.,-1.));
#13433=DIRECTION('ref_axis',(-1.,0.,0.));
#13434=DIRECTION('',(0.,-1.,0.));
#13435=DIRECTION('',(0.,1.,0.));
#13436=DIRECTION('',(1.,0.,0.));
#13437=DIRECTION('center_axis',(0.,-1.,0.));
#13438=DIRECTION('ref_axis',(0.,0.,-1.));
#13439=DIRECTION('center_axis',(0.,-1.,0.));
#13440=DIRECTION('ref_axis',(1.,0.,0.));
#13441=DIRECTION('center_axis',(0.,1.,0.));
#13442=DIRECTION('ref_axis',(1.,0.,0.));
#13443=DIRECTION('',(-1.,0.,0.));
#13444=DIRECTION('center_axis',(0.,0.,1.));
#13445=DIRECTION('ref_axis',(1.,0.,0.));
#13446=DIRECTION('',(0.,1.,0.));
#13447=DIRECTION('',(0.,-1.,0.));
#13448=DIRECTION('center_axis',(0.,1.,0.));
#13449=DIRECTION('ref_axis',(0.,0.,1.));
#13450=DIRECTION('center_axis',(0.,-1.,0.));
#13451=DIRECTION('ref_axis',(1.,0.,0.));
#13452=DIRECTION('center_axis',(0.,-1.,0.));
#13453=DIRECTION('ref_axis',(1.,0.,0.));
#13454=DIRECTION('center_axis',(0.,-1.,0.));
#13455=DIRECTION('ref_axis',(1.,0.,0.));
#13456=DIRECTION('center_axis',(0.,-1.,0.));
#13457=DIRECTION('ref_axis',(1.,0.,0.));
#13458=DIRECTION('',(0.,1.,0.));
#13459=DIRECTION('center_axis',(0.,-1.,0.));
#13460=DIRECTION('ref_axis',(0.,0.,-1.));
#13461=DIRECTION('center_axis',(0.,-1.,0.));
#13462=DIRECTION('ref_axis',(1.,0.,0.));
#13463=DIRECTION('center_axis',(0.,-1.,0.));
#13464=DIRECTION('ref_axis',(1.,0.,0.));
#13465=DIRECTION('',(0.,1.,0.));
#13466=DIRECTION('',(0.,0.,1.));
#13467=DIRECTION('',(1.,0.,0.));
#13468=DIRECTION('',(0.,0.,1.));
#13469=DIRECTION('',(1.,0.,0.));
#13470=DIRECTION('axis',(0.,0.,1.));
#13471=DIRECTION('refdir',(1.,0.,0.));
#13472=DIRECTION('center_axis',(0.866025403784439,0.,-0.5));
#13473=DIRECTION('ref_axis',(0.5,0.,0.866025403784439));
#13474=DIRECTION('',(-0.5,0.,-0.866025403784439));
#13475=DIRECTION('',(0.,-1.,0.));
#13476=DIRECTION('',(0.5,0.,0.866025403784439));
#13477=DIRECTION('',(0.,-1.,0.));
#13478=DIRECTION('center_axis',(1.60246890531964E-16,0.,-1.));
#13479=DIRECTION('ref_axis',(1.,0.,1.60246890531964E-16));
#13480=DIRECTION('',(-1.,0.,-1.60246890531964E-16));
#13481=DIRECTION('',(0.,-1.,0.));
#13482=DIRECTION('',(1.,0.,1.60246890531964E-16));
#13483=DIRECTION('center_axis',(-0.866025403784439,0.,-0.5));
#13484=DIRECTION('ref_axis',(0.5,0.,-0.866025403784439));
#13485=DIRECTION('',(-0.5,0.,0.866025403784439));
#13486=DIRECTION('',(0.,-1.,0.));
#13487=DIRECTION('',(0.5,0.,-0.866025403784439));
#13488=DIRECTION('center_axis',(-0.866025403784439,0.,0.5));
#13489=DIRECTION('ref_axis',(-0.5,0.,-0.866025403784439));
#13490=DIRECTION('',(0.5,0.,0.866025403784439));
#13491=DIRECTION('',(0.,-1.,0.));
#13492=DIRECTION('',(-0.5,0.,-0.866025403784439));
#13493=DIRECTION('center_axis',(-1.60246890531964E-16,0.,1.));
#13494=DIRECTION('ref_axis',(-1.,0.,-1.60246890531964E-16));
#13495=DIRECTION('',(1.,0.,1.60246890531964E-16));
#13496=DIRECTION('',(0.,-1.,0.));
#13497=DIRECTION('',(-1.,0.,-1.60246890531964E-16));
#13498=DIRECTION('center_axis',(0.866025403784439,0.,0.5));
#13499=DIRECTION('ref_axis',(-0.5,0.,0.866025403784439));
#13500=DIRECTION('',(0.5,0.,-0.866025403784439));
#13501=DIRECTION('',(-0.5,0.,0.866025403784439));
#13502=DIRECTION('center_axis',(0.,1.,0.));
#13503=DIRECTION('ref_axis',(1.,0.,0.));
#13504=DIRECTION('center_axis',(0.,-1.,0.));
#13505=DIRECTION('ref_axis',(0.,0.,-1.));
#13506=DIRECTION('center_axis',(0.,1.,0.));
#13507=DIRECTION('ref_axis',(1.,0.,0.));
#13508=DIRECTION('center_axis',(0.,1.,0.));
#13509=DIRECTION('ref_axis',(1.,0.,0.));
#13510=DIRECTION('center_axis',(0.,1.,0.));
#13511=DIRECTION('ref_axis',(0.,0.,1.));
#13512=DIRECTION('center_axis',(0.,-1.,0.));
#13513=DIRECTION('ref_axis',(1.,0.,0.));
#13514=DIRECTION('center_axis',(0.,-1.,0.));
#13515=DIRECTION('ref_axis',(1.,0.,0.));
#13516=DIRECTION('center_axis',(0.,-1.,0.));
#13517=DIRECTION('ref_axis',(1.,0.,0.));
#13518=DIRECTION('',(0.707106781186547,0.707106781186548,8.65956056235493E-17));
#13519=DIRECTION('center_axis',(0.,-1.,0.));
#13520=DIRECTION('ref_axis',(1.,0.,0.));
#13521=DIRECTION('center_axis',(0.,-1.,0.));
#13522=DIRECTION('ref_axis',(1.,0.,0.));
#13523=DIRECTION('',(0.,1.,0.));
#13524=DIRECTION('center_axis',(0.,1.,0.));
#13525=DIRECTION('ref_axis',(1.,0.,0.));
#13526=DIRECTION('center_axis',(0.,-1.,0.));
#13527=DIRECTION('ref_axis',(1.,0.,0.));
#13528=DIRECTION('',(-0.707106781186547,0.707106781186548,-8.65956056235493E-17));
#13529=DIRECTION('center_axis',(0.,-1.,0.));
#13530=DIRECTION('ref_axis',(0.,0.,-1.));
#13531=DIRECTION('center_axis',(0.,-1.,0.));
#13532=DIRECTION('ref_axis',(1.,0.,0.));
#13533=DIRECTION('center_axis',(0.,1.,0.));
#13534=DIRECTION('ref_axis',(1.,0.,0.));
#13535=DIRECTION('center_axis',(0.,1.,0.));
#13536=DIRECTION('ref_axis',(1.,0.,0.));
#13537=DIRECTION('',(-0.447213595499958,0.894427190999916,-5.47678698264203E-17));
#13538=DIRECTION('center_axis',(0.,-1.,0.));
#13539=DIRECTION('ref_axis',(1.,0.,0.));
#13540=DIRECTION('',(0.,1.,0.));
#13541=DIRECTION('',(0.,0.,1.));
#13542=DIRECTION('',(1.,0.,0.));
#13543=DIRECTION('',(0.,0.,1.));
#13544=DIRECTION('',(1.,0.,0.));
#13545=DIRECTION('',(0.,0.,1.));
#13546=DIRECTION('',(1.,0.,0.));
#13547=DIRECTION('',(0.,0.,1.));
#13548=DIRECTION('',(1.,0.,0.));
#13549=DIRECTION('',(0.,0.,1.));
#13550=DIRECTION('',(1.,0.,0.));
#13551=DIRECTION('',(0.,0.,1.));
#13552=DIRECTION('',(1.,0.,0.));
#13553=DIRECTION('',(0.,0.,1.));
#13554=DIRECTION('',(1.,0.,0.));
#13555=DIRECTION('',(0.,0.,1.));
#13556=DIRECTION('',(1.,0.,0.));
#13557=DIRECTION('',(0.,0.,1.));
#13558=DIRECTION('',(1.,0.,0.));
#13559=DIRECTION('',(0.,0.,1.));
#13560=DIRECTION('',(1.,0.,0.));
#13561=DIRECTION('',(0.,0.,1.));
#13562=DIRECTION('',(1.,0.,0.));
#13563=DIRECTION('',(0.,-1.,2.22044604925031E-16));
#13564=DIRECTION('',(1.,0.,0.));
#13565=DIRECTION('',(0.,-1.,2.22044604925031E-16));
#13566=DIRECTION('',(1.,0.,0.));
#13567=DIRECTION('',(0.,-1.,2.22044604925031E-16));
#13568=DIRECTION('',(1.,0.,0.));
#13569=DIRECTION('',(0.,-1.,2.22044604925031E-16));
#13570=DIRECTION('',(1.,0.,0.));
#13571=DIRECTION('',(0.,0.,1.));
#13572=DIRECTION('',(1.,0.,0.));
#13573=DIRECTION('',(0.,-1.,2.22044604925031E-16));
#13574=DIRECTION('',(1.,0.,0.));
#13575=DIRECTION('',(0.,-1.,2.22044604925031E-16));
#13576=DIRECTION('',(1.,0.,0.));
#13577=DIRECTION('',(0.,-1.,2.22044604925031E-16));
#13578=DIRECTION('',(1.,0.,0.));
#13579=DIRECTION('',(0.,-1.,2.22044604925031E-16));
#13580=DIRECTION('',(1.,0.,0.));
#13581=DIRECTION('',(0.,-1.,2.22044604925031E-16));
#13582=DIRECTION('',(1.,0.,0.));
#13583=DIRECTION('',(0.,-1.,2.22044604925031E-16));
#13584=DIRECTION('',(1.,0.,0.));
#13585=DIRECTION('',(0.,-1.,2.22044604925031E-16));
#13586=DIRECTION('',(1.,0.,0.));
#13587=DIRECTION('',(0.,-1.,2.22044604925031E-16));
#13588=DIRECTION('',(1.,0.,0.));
#13589=DIRECTION('',(0.,0.,1.));
#13590=DIRECTION('',(1.,0.,0.));
#13591=DIRECTION('',(0.,-1.,2.22044604925031E-16));
#13592=DIRECTION('',(1.,0.,0.));
#13593=DIRECTION('',(0.,-1.,2.22044604925031E-16));
#13594=DIRECTION('',(1.,0.,0.));
#13595=DIRECTION('',(0.,-1.,2.22044604925031E-16));
#13596=DIRECTION('',(1.,0.,0.));
#13597=DIRECTION('',(0.,-1.,2.22044604925031E-16));
#13598=DIRECTION('',(1.,0.,0.));
#13599=DIRECTION('',(0.,0.,1.));
#13600=DIRECTION('',(2.22044604925031E-16,-1.,0.));
#13601=DIRECTION('',(0.,-1.,2.22044604925031E-16));
#13602=DIRECTION('',(1.,0.,0.));
#13603=DIRECTION('',(0.,-1.,2.22044604925031E-16));
#13604=DIRECTION('',(1.,0.,0.));
#13605=DIRECTION('',(0.,-1.,2.22044604925031E-16));
#13606=DIRECTION('',(1.,0.,0.));
#13607=DIRECTION('',(0.,-1.,2.22044604925031E-16));
#13608=DIRECTION('',(1.,0.,0.));
#13609=DIRECTION('',(0.,0.,1.));
#13610=DIRECTION('',(-1.,1.22464679914735E-16,0.));
#13611=DIRECTION('',(0.,0.,1.));
#13612=DIRECTION('',(2.22044604925031E-16,-1.,0.));
#13613=DIRECTION('',(0.,-1.,2.22044604925031E-16));
#13614=DIRECTION('',(1.,0.,0.));
#13615=DIRECTION('',(0.,-1.,2.22044604925031E-16));
#13616=DIRECTION('',(1.,0.,0.));
#13617=DIRECTION('',(0.,-1.,2.22044604925031E-16));
#13618=DIRECTION('',(1.,0.,0.));
#13619=DIRECTION('',(0.,-1.,2.22044604925031E-16));
#13620=DIRECTION('',(1.,0.,0.));
#13621=DIRECTION('',(0.,0.,1.));
#13622=DIRECTION('',(-1.,1.22464679914735E-16,0.));
#13623=DIRECTION('',(0.,-1.,2.22044604925031E-16));
#13624=DIRECTION('',(1.,0.,0.));
#13625=DIRECTION('',(0.,-1.,2.22044604925031E-16));
#13626=DIRECTION('',(1.,0.,0.));
#13627=DIRECTION('',(0.,0.,1.));
#13628=DIRECTION('',(2.22044604925031E-16,-1.,0.));
#13629=DIRECTION('',(0.,-1.,2.22044604925031E-16));
#13630=DIRECTION('',(1.,0.,0.));
#13631=DIRECTION('',(0.,-1.,2.22044604925031E-16));
#13632=DIRECTION('',(1.,0.,0.));
#13633=DIRECTION('',(0.,-1.,2.22044604925031E-16));
#13634=DIRECTION('',(1.,0.,0.));
#13635=DIRECTION('',(0.,-1.,2.22044604925031E-16));
#13636=DIRECTION('',(1.,0.,0.));
#13637=DIRECTION('',(0.,0.,1.));
#13638=DIRECTION('',(-1.,1.22464679914735E-16,0.));
#13639=DIRECTION('',(0.,0.,1.));
#13640=DIRECTION('',(2.22044604925031E-16,-1.,0.));
#13641=DIRECTION('',(0.,-1.,2.22044604925031E-16));
#13642=DIRECTION('',(1.,0.,0.));
#13643=DIRECTION('',(0.,-1.,2.22044604925031E-16));
#13644=DIRECTION('',(1.,0.,0.));
#13645=DIRECTION('',(0.,-1.,2.22044604925031E-16));
#13646=DIRECTION('',(1.,0.,0.));
#13647=DIRECTION('',(0.,-1.,2.22044604925031E-16));
#13648=DIRECTION('',(1.,0.,0.));
#13649=DIRECTION('',(0.,0.,1.));
#13650=DIRECTION('',(-1.,1.22464679914735E-16,0.));
#13651=DIRECTION('',(0.,-1.,2.22044604925031E-16));
#13652=DIRECTION('',(1.,0.,0.));
#13653=DIRECTION('',(0.,-1.,2.22044604925031E-16));
#13654=DIRECTION('',(1.,0.,0.));
#13655=DIRECTION('',(0.,0.,1.));
#13656=DIRECTION('',(1.,0.,0.));
#13657=DIRECTION('',(0.,0.,1.));
#13658=DIRECTION('',(1.,0.,0.));
#13659=DIRECTION('',(0.,0.,1.));
#13660=DIRECTION('',(1.,0.,0.));
#13661=DIRECTION('',(0.,0.,1.));
#13662=DIRECTION('',(1.,0.,0.));
#13663=DIRECTION('',(0.,0.,1.));
#13664=DIRECTION('',(1.,0.,0.));
#13665=DIRECTION('',(0.,0.,1.));
#13666=DIRECTION('',(1.,0.,0.));
#13667=DIRECTION('',(0.,0.,1.));
#13668=DIRECTION('',(1.,0.,0.));
#13669=DIRECTION('',(0.,0.,1.));
#13670=DIRECTION('',(1.,0.,0.));
#13671=DIRECTION('',(0.,0.,1.));
#13672=DIRECTION('',(1.,0.,0.));
#13673=DIRECTION('',(0.,0.,1.));
#13674=DIRECTION('',(1.,0.,0.));
#13675=DIRECTION('',(0.,0.,1.));
#13676=DIRECTION('',(1.,0.,0.));
#13677=DIRECTION('',(8.65956056235493E-17,-8.65956056235493E-17,-1.));
#13678=DIRECTION('',(2.22044604925031E-16,1.,-8.65956056235494E-17));
#13679=DIRECTION('',(0.,-1.,2.22044604925031E-16));
#13680=DIRECTION('',(1.,0.,0.));
#13681=DIRECTION('',(0.,-1.,2.22044604925031E-16));
#13682=DIRECTION('',(1.,0.,0.));
#13683=DIRECTION('',(0.,-1.,2.22044604925031E-16));
#13684=DIRECTION('',(1.,0.,0.));
#13685=DIRECTION('',(0.,0.,1.));
#13686=DIRECTION('',(1.,0.,0.));
#13687=DIRECTION('',(0.,0.,1.));
#13688=DIRECTION('',(1.,0.,0.));
#13689=DIRECTION('',(0.,0.,1.));
#13690=DIRECTION('',(1.,0.,0.));
#13691=DIRECTION('',(0.,0.,1.));
#13692=DIRECTION('',(1.,0.,0.));
#13693=DIRECTION('',(0.,0.,1.));
#13694=DIRECTION('',(1.,0.,0.));
#13695=DIRECTION('',(0.,0.,1.));
#13696=DIRECTION('',(1.,0.,0.));
#13697=DIRECTION('',(0.,0.,1.));
#13698=DIRECTION('',(1.,0.,0.));
#13699=DIRECTION('',(0.,0.,1.));
#13700=DIRECTION('',(1.,0.,0.));
#13701=DIRECTION('',(0.,0.,1.));
#13702=DIRECTION('',(2.22044604925031E-16,-1.,0.));
#13703=DIRECTION('',(0.,0.,1.));
#13704=DIRECTION('',(2.22044604925031E-16,-1.,0.));
#13705=DIRECTION('',(0.,0.,1.));
#13706=DIRECTION('',(2.22044604925031E-16,1.,0.));
#13707=DIRECTION('',(0.,0.,1.));
#13708=DIRECTION('',(2.22044604925031E-16,1.,0.));
#13709=DIRECTION('',(0.,0.,1.));
#13710=DIRECTION('',(2.22044604925031E-16,1.,0.));
#13711=DIRECTION('',(0.,0.,1.));
#13712=DIRECTION('',(2.22044604925031E-16,1.,0.));
#13713=DIRECTION('',(0.,0.,1.));
#13714=DIRECTION('',(2.22044604925031E-16,-1.,0.));
#13715=DIRECTION('',(0.,0.,1.));
#13716=DIRECTION('',(2.22044604925031E-16,-1.,0.));
#13717=DIRECTION('',(0.,0.,1.));
#13718=DIRECTION('',(2.22044604925031E-16,-1.,0.));
#13719=DIRECTION('',(0.,0.,1.));
#13720=DIRECTION('',(2.22044604925031E-16,-1.,0.));
#13721=DIRECTION('',(0.,0.,1.));
#13722=DIRECTION('',(1.,0.,0.));
#13723=DIRECTION('',(0.,0.,1.));
#13724=DIRECTION('',(1.,0.,0.));
#13725=DIRECTION('',(0.,0.,1.));
#13726=DIRECTION('',(1.,0.,0.));
#13727=DIRECTION('',(0.,0.,1.));
#13728=DIRECTION('',(1.,0.,0.));
#13729=DIRECTION('',(0.,0.,1.));
#13730=DIRECTION('',(1.,0.,0.));
#13731=CARTESIAN_POINT('',(0.,0.,0.));
#13732=CARTESIAN_POINT('',(0.,0.,0.));
#13733=CARTESIAN_POINT('',(0.,0.,0.));
#13734=CARTESIAN_POINT('Origin',(19.2,0.,-0.1));
#13735=CARTESIAN_POINT('',(19.035,-2.02066721859312E-17,0.));
#13736=CARTESIAN_POINT('Origin',(19.2,0.,0.));
#13737=CARTESIAN_POINT('',(19.035,2.02066721859312E-17,1.));
#13738=CARTESIAN_POINT('',(19.035,-2.02066721859312E-17,-0.1));
#13739=CARTESIAN_POINT('Origin',(19.2,0.,1.));
#13740=CARTESIAN_POINT('Origin',(20.8,0.,-0.1));
#13741=CARTESIAN_POINT('',(20.635,-2.02066721859312E-17,0.));
#13742=CARTESIAN_POINT('Origin',(20.8,0.,0.));
#13743=CARTESIAN_POINT('',(20.635,2.02066721859312E-17,1.));
#13744=CARTESIAN_POINT('',(20.635,-2.02066721859312E-17,-0.1));
#13745=CARTESIAN_POINT('Origin',(20.8,0.,1.));
#13746=CARTESIAN_POINT('Origin',(3.2,0.,-0.1));
#13747=CARTESIAN_POINT('',(3.035,-2.02066721859313E-17,0.));
#13748=CARTESIAN_POINT('Origin',(3.2,0.,0.));
#13749=CARTESIAN_POINT('',(3.035,2.02066721859313E-17,1.));
#13750=CARTESIAN_POINT('',(3.035,-2.02066721859313E-17,-0.1));
#13751=CARTESIAN_POINT('Origin',(3.2,0.,1.));
#13752=CARTESIAN_POINT('Origin',(4.8,0.,-0.1));
#13753=CARTESIAN_POINT('',(4.635,-2.02066721859313E-17,0.));
#13754=CARTESIAN_POINT('Origin',(4.8,0.,0.));
#13755=CARTESIAN_POINT('',(4.635,2.02066721859313E-17,1.));
#13756=CARTESIAN_POINT('',(4.635,-2.02066721859313E-17,-0.1));
#13757=CARTESIAN_POINT('Origin',(4.8,0.,1.));
#13758=CARTESIAN_POINT('Origin',(5.8,-8.5,-0.1));
#13759=CARTESIAN_POINT('',(5.59,-8.5,0.));
#13760=CARTESIAN_POINT('Origin',(5.8,-8.5,0.));
#13761=CARTESIAN_POINT('',(5.59,-8.5,1.));
#13762=CARTESIAN_POINT('',(5.59,-8.5,-0.1));
#13763=CARTESIAN_POINT('Origin',(5.8,-8.5,1.));
#13764=CARTESIAN_POINT('Origin',(-5.8,-5.5,-0.1));
#13765=CARTESIAN_POINT('',(-6.01,-5.5,0.));
#13766=CARTESIAN_POINT('Origin',(-5.8,-5.5,0.));
#13767=CARTESIAN_POINT('',(-6.01,-5.5,1.));
#13768=CARTESIAN_POINT('',(-6.01,-5.5,-0.1));
#13769=CARTESIAN_POINT('Origin',(-5.8,-5.5,1.));
#13770=CARTESIAN_POINT('Origin',(-5.8,-8.5,-0.1));
#13771=CARTESIAN_POINT('',(-6.01,-8.5,0.));
#13772=CARTESIAN_POINT('Origin',(-5.8,-8.5,0.));
#13773=CARTESIAN_POINT('',(-6.01,-8.5,1.));
#13774=CARTESIAN_POINT('',(-6.01,-8.5,-0.1));
#13775=CARTESIAN_POINT('Origin',(-5.8,-8.5,1.));
#13776=CARTESIAN_POINT('Origin',(5.8,-5.5,-0.1));
#13777=CARTESIAN_POINT('',(5.59,-5.5,0.));
#13778=CARTESIAN_POINT('Origin',(5.8,-5.5,0.));
#13779=CARTESIAN_POINT('',(5.59,-5.5,1.));
#13780=CARTESIAN_POINT('',(5.59,-5.5,-0.1));
#13781=CARTESIAN_POINT('Origin',(5.8,-5.5,1.));
#13782=CARTESIAN_POINT('Origin',(5.8,-16.5,-0.1));
#13783=CARTESIAN_POINT('',(5.59,-16.5,0.));
#13784=CARTESIAN_POINT('Origin',(5.8,-16.5,0.));
#13785=CARTESIAN_POINT('',(5.59,-16.5,1.));
#13786=CARTESIAN_POINT('',(5.59,-16.5,-0.1));
#13787=CARTESIAN_POINT('Origin',(5.8,-16.5,1.));
#13788=CARTESIAN_POINT('Origin',(-5.8,-13.5,-0.1));
#13789=CARTESIAN_POINT('',(-6.01,-13.5,0.));
#13790=CARTESIAN_POINT('Origin',(-5.8,-13.5,0.));
#13791=CARTESIAN_POINT('',(-6.01,-13.5,1.));
#13792=CARTESIAN_POINT('',(-6.01,-13.5,-0.1));
#13793=CARTESIAN_POINT('Origin',(-5.8,-13.5,1.));
#13794=CARTESIAN_POINT('Origin',(-5.8,-16.5,-0.1));
#13795=CARTESIAN_POINT('',(-6.01,-16.5,0.));
#13796=CARTESIAN_POINT('Origin',(-5.8,-16.5,0.));
#13797=CARTESIAN_POINT('',(-6.01,-16.5,1.));
#13798=CARTESIAN_POINT('',(-6.01,-16.5,-0.1));
#13799=CARTESIAN_POINT('Origin',(-5.8,-16.5,1.));
#13800=CARTESIAN_POINT('Origin',(5.8,-13.5,-0.1));
#13801=CARTESIAN_POINT('',(5.59,-13.5,0.));
#13802=CARTESIAN_POINT('Origin',(5.8,-13.5,0.));
#13803=CARTESIAN_POINT('',(5.59,-13.5,1.));
#13804=CARTESIAN_POINT('',(5.59,-13.5,-0.1));
#13805=CARTESIAN_POINT('Origin',(5.8,-13.5,1.));
#13806=CARTESIAN_POINT('Origin',(24.,9.,0.));
#13807=CARTESIAN_POINT('',(24.,9.,0.));
#13808=CARTESIAN_POINT('',(-8.,9.,0.));
#13809=CARTESIAN_POINT('',(24.,9.,0.));
#13810=CARTESIAN_POINT('',(-8.,9.,1.));
#13811=CARTESIAN_POINT('',(-8.,9.,0.));
#13812=CARTESIAN_POINT('',(24.,9.,1.));
#13813=CARTESIAN_POINT('',(24.,9.,1.));
#13814=CARTESIAN_POINT('',(24.,9.,0.));
#13815=CARTESIAN_POINT('Origin',(24.,-18.,0.));
#13816=CARTESIAN_POINT('',(24.,-18.,0.));
#13817=CARTESIAN_POINT('',(24.,-18.,0.));
#13818=CARTESIAN_POINT('',(24.,-18.,1.));
#13819=CARTESIAN_POINT('',(24.,-18.,1.));
#13820=CARTESIAN_POINT('',(24.,-18.,0.));
#13821=CARTESIAN_POINT('Origin',(-8.,-18.,0.));
#13822=CARTESIAN_POINT('',(-8.,-18.,0.));
#13823=CARTESIAN_POINT('',(-8.,-18.,0.));
#13824=CARTESIAN_POINT('',(-8.,-18.,1.));
#13825=CARTESIAN_POINT('',(-8.,-18.,1.));
#13826=CARTESIAN_POINT('',(-8.,-18.,0.));
#13827=CARTESIAN_POINT('Origin',(-8.,9.,0.));
#13828=CARTESIAN_POINT('',(-8.,9.,0.));
#13829=CARTESIAN_POINT('',(-8.,9.,1.));
#13830=CARTESIAN_POINT('Origin',(8.,-4.5,1.));
#13831=CARTESIAN_POINT('Origin',(8.,-4.5,0.));
#13832=CARTESIAN_POINT('',(0.,0.,0.));
#13833=CARTESIAN_POINT('Origin',(-4.75,-15.,5.3));
#13834=CARTESIAN_POINT('',(-5.09,-15.,5.3));
#13835=CARTESIAN_POINT('Origin',(-4.75,-15.,5.3));
#13836=CARTESIAN_POINT('',(-5.09,-15.,6.67));
#13837=CARTESIAN_POINT('',(-5.09,-15.,5.3));
#13838=CARTESIAN_POINT('Origin',(-4.75,-15.,6.67));
#13839=CARTESIAN_POINT('Origin',(-4.75,-15.,5.3));
#13840=CARTESIAN_POINT('Origin',(4.75,-15.,5.3));
#13841=CARTESIAN_POINT('',(4.41,-15.,5.3));
#13842=CARTESIAN_POINT('Origin',(4.75,-15.,5.3));
#13843=CARTESIAN_POINT('',(4.41,-15.,6.67));
#13844=CARTESIAN_POINT('',(4.41,-15.,5.3));
#13845=CARTESIAN_POINT('Origin',(4.75,-15.,6.67));
#13846=CARTESIAN_POINT('Origin',(4.75,-15.,5.3));
#13847=CARTESIAN_POINT('Origin',(5.8,-16.5,2.2));
#13848=CARTESIAN_POINT('',(5.3,-16.5,2.2));
#13849=CARTESIAN_POINT('Origin',(5.8,-16.5,2.2));
#13850=CARTESIAN_POINT('',(5.3,-16.5,6.67));
#13851=CARTESIAN_POINT('',(5.3,-16.5,2.2));
#13852=CARTESIAN_POINT('Origin',(5.8,-16.5,6.67));
#13853=CARTESIAN_POINT('Origin',(5.8,-16.5,2.2));
#13854=CARTESIAN_POINT('',(5.525,-16.5,2.2));
#13855=CARTESIAN_POINT('Origin',(5.8,-16.5,2.2));
#13856=CARTESIAN_POINT('Origin',(-5.8,-13.5,2.2));
#13857=CARTESIAN_POINT('',(-6.3,-13.5,2.2));
#13858=CARTESIAN_POINT('Origin',(-5.8,-13.5,2.2));
#13859=CARTESIAN_POINT('',(-6.3,-13.5,6.67));
#13860=CARTESIAN_POINT('',(-6.3,-13.5,2.2));
#13861=CARTESIAN_POINT('Origin',(-5.8,-13.5,6.67));
#13862=CARTESIAN_POINT('Origin',(-5.8,-13.5,2.2));
#13863=CARTESIAN_POINT('',(-6.075,-13.5,2.2));
#13864=CARTESIAN_POINT('Origin',(-5.8,-13.5,2.2));
#13865=CARTESIAN_POINT('Origin',(-5.8,-16.5,2.2));
#13866=CARTESIAN_POINT('',(-6.3,-16.5,2.2));
#13867=CARTESIAN_POINT('Origin',(-5.8,-16.5,2.2));
#13868=CARTESIAN_POINT('',(-6.3,-16.5,6.67));
#13869=CARTESIAN_POINT('',(-6.3,-16.5,2.2));
#13870=CARTESIAN_POINT('Origin',(-5.8,-16.5,6.67));
#13871=CARTESIAN_POINT('Origin',(-5.8,-16.5,2.2));
#13872=CARTESIAN_POINT('',(-6.075,-16.5,2.2));
#13873=CARTESIAN_POINT('Origin',(-5.8,-16.5,2.2));
#13874=CARTESIAN_POINT('Origin',(5.8,-13.5,2.2));
#13875=CARTESIAN_POINT('',(5.3,-13.5,2.2));
#13876=CARTESIAN_POINT('Origin',(5.8,-13.5,2.2));
#13877=CARTESIAN_POINT('',(5.3,-13.5,6.67));
#13878=CARTESIAN_POINT('',(5.3,-13.5,2.2));
#13879=CARTESIAN_POINT('Origin',(5.8,-13.5,6.67));
#13880=CARTESIAN_POINT('Origin',(5.8,-13.5,2.2));
#13881=CARTESIAN_POINT('',(5.525,-13.5,2.2));
#13882=CARTESIAN_POINT('Origin',(5.8,-13.5,2.2));
#13883=CARTESIAN_POINT('Origin',(5.8,-16.5,0.9));
#13884=CARTESIAN_POINT('',(5.525,-16.5,1.));
#13885=CARTESIAN_POINT('Origin',(5.8,-16.5,1.));
#13886=CARTESIAN_POINT('',(5.525,-16.5,0.9));
#13887=CARTESIAN_POINT('Origin',(-5.8,-13.5,0.9));
#13888=CARTESIAN_POINT('',(-6.075,-13.5,1.));
#13889=CARTESIAN_POINT('Origin',(-5.8,-13.5,1.));
#13890=CARTESIAN_POINT('',(-6.075,-13.5,0.9));
#13891=CARTESIAN_POINT('Origin',(-5.8,-16.5,0.9));
#13892=CARTESIAN_POINT('',(-6.075,-16.5,1.));
#13893=CARTESIAN_POINT('Origin',(-5.8,-16.5,1.));
#13894=CARTESIAN_POINT('',(-6.075,-16.5,0.9));
#13895=CARTESIAN_POINT('Origin',(5.8,-13.5,0.9));
#13896=CARTESIAN_POINT('',(5.525,-13.5,1.));
#13897=CARTESIAN_POINT('Origin',(5.8,-13.5,1.));
#13898=CARTESIAN_POINT('',(5.525,-13.5,0.9));
#13899=CARTESIAN_POINT('Origin',(7.,-12.75,1.));
#13900=CARTESIAN_POINT('',(7.,-12.75,1.));
#13901=CARTESIAN_POINT('',(-7.,-12.75,1.));
#13902=CARTESIAN_POINT('',(7.,-12.75,1.));
#13903=CARTESIAN_POINT('',(-7.,-12.75,6.67));
#13904=CARTESIAN_POINT('',(-7.,-12.75,1.));
#13905=CARTESIAN_POINT('',(7.,-12.75,6.67));
#13906=CARTESIAN_POINT('',(7.,-12.75,6.67));
#13907=CARTESIAN_POINT('',(7.,-12.75,1.));
#13908=CARTESIAN_POINT('Origin',(7.,-17.25,1.));
#13909=CARTESIAN_POINT('',(7.,-17.25,1.));
#13910=CARTESIAN_POINT('',(7.,-17.25,1.));
#13911=CARTESIAN_POINT('',(7.,-17.25,6.67));
#13912=CARTESIAN_POINT('',(7.,-17.25,6.67));
#13913=CARTESIAN_POINT('',(7.,-17.25,1.));
#13914=CARTESIAN_POINT('Origin',(-7.,-17.25,1.));
#13915=CARTESIAN_POINT('',(-7.,-17.25,1.));
#13916=CARTESIAN_POINT('',(-7.,-17.25,1.));
#13917=CARTESIAN_POINT('',(-7.,-17.25,6.67));
#13918=CARTESIAN_POINT('',(-7.,-17.25,6.67));
#13919=CARTESIAN_POINT('',(-7.,-17.25,1.));
#13920=CARTESIAN_POINT('Origin',(-7.,-12.75,1.));
#13921=CARTESIAN_POINT('',(-7.,-12.75,1.));
#13922=CARTESIAN_POINT('',(-7.,-12.75,6.67));
#13923=CARTESIAN_POINT('Origin',(0.,-15.,6.67));
#13924=CARTESIAN_POINT('Origin',(0.,-15.,1.));
#13925=CARTESIAN_POINT('',(0.,0.,0.));
#13926=CARTESIAN_POINT('Origin',(-4.75,-15.,6.67));
#13927=CARTESIAN_POINT('',(-5.175,-15.,7.87));
#13928=CARTESIAN_POINT('Origin',(-4.75,-15.,7.87));
#13929=CARTESIAN_POINT('',(-5.175,-15.,6.67));
#13930=CARTESIAN_POINT('',(-5.175,-15.,6.67));
#13931=CARTESIAN_POINT('Origin',(-4.75,-15.,6.67));
#13932=CARTESIAN_POINT('Origin',(-4.75,-15.,6.67));
#13933=CARTESIAN_POINT('',(-5.395,-15.,7.87));
#13934=CARTESIAN_POINT('Origin',(-4.75,-15.,7.87));
#13935=CARTESIAN_POINT('',(-5.395,-15.,6.67));
#13936=CARTESIAN_POINT('',(-5.395,-15.,6.67));
#13937=CARTESIAN_POINT('Origin',(-4.75,-15.,6.67));
#13938=CARTESIAN_POINT('Origin',(-4.75,-15.,7.87));
#13939=CARTESIAN_POINT('Origin',(-4.75,-15.,6.67));
#13940=CARTESIAN_POINT('',(0.,0.,0.));
#13941=CARTESIAN_POINT('Origin',(4.75,-15.,6.67));
#13942=CARTESIAN_POINT('',(4.325,-15.,7.87));
#13943=CARTESIAN_POINT('Origin',(4.75,-15.,7.87));
#13944=CARTESIAN_POINT('',(4.325,-15.,6.67));
#13945=CARTESIAN_POINT('',(4.325,-15.,6.67));
#13946=CARTESIAN_POINT('Origin',(4.75,-15.,6.67));
#13947=CARTESIAN_POINT('Origin',(4.75,-15.,6.67));
#13948=CARTESIAN_POINT('',(4.105,-15.,7.87));
#13949=CARTESIAN_POINT('Origin',(4.75,-15.,7.87));
#13950=CARTESIAN_POINT('',(4.105,-15.,6.67));
#13951=CARTESIAN_POINT('',(4.105,-15.,6.67));
#13952=CARTESIAN_POINT('Origin',(4.75,-15.,6.67));
#13953=CARTESIAN_POINT('Origin',(4.75,-15.,7.87));
#13954=CARTESIAN_POINT('Origin',(4.75,-15.,6.67));
#13955=CARTESIAN_POINT('',(0.,0.,0.));
#13956=CARTESIAN_POINT('Origin',(-4.75,-7.,5.3));
#13957=CARTESIAN_POINT('',(-5.09,-7.,5.3));
#13958=CARTESIAN_POINT('Origin',(-4.75,-7.,5.3));
#13959=CARTESIAN_POINT('',(-5.09,-7.,6.67));
#13960=CARTESIAN_POINT('',(-5.09,-7.,5.3));
#13961=CARTESIAN_POINT('Origin',(-4.75,-7.,6.67));
#13962=CARTESIAN_POINT('Origin',(-4.75,-7.,5.3));
#13963=CARTESIAN_POINT('Origin',(4.75,-7.,5.3));
#13964=CARTESIAN_POINT('',(4.41,-7.,5.3));
#13965=CARTESIAN_POINT('Origin',(4.75,-7.,5.3));
#13966=CARTESIAN_POINT('',(4.41,-7.,6.67));
#13967=CARTESIAN_POINT('',(4.41,-7.,5.3));
#13968=CARTESIAN_POINT('Origin',(4.75,-7.,6.67));
#13969=CARTESIAN_POINT('Origin',(4.75,-7.,5.3));
#13970=CARTESIAN_POINT('Origin',(5.8,-8.5,2.2));
#13971=CARTESIAN_POINT('',(5.3,-8.5,2.2));
#13972=CARTESIAN_POINT('Origin',(5.8,-8.5,2.2));
#13973=CARTESIAN_POINT('',(5.3,-8.5,6.67));
#13974=CARTESIAN_POINT('',(5.3,-8.5,2.2));
#13975=CARTESIAN_POINT('Origin',(5.8,-8.5,6.67));
#13976=CARTESIAN_POINT('Origin',(5.8,-8.5,2.2));
#13977=CARTESIAN_POINT('',(5.525,-8.5,2.2));
#13978=CARTESIAN_POINT('Origin',(5.8,-8.5,2.2));
#13979=CARTESIAN_POINT('Origin',(-5.8,-5.5,2.2));
#13980=CARTESIAN_POINT('',(-6.3,-5.5,2.2));
#13981=CARTESIAN_POINT('Origin',(-5.8,-5.5,2.2));
#13982=CARTESIAN_POINT('',(-6.3,-5.5,6.67));
#13983=CARTESIAN_POINT('',(-6.3,-5.5,2.2));
#13984=CARTESIAN_POINT('Origin',(-5.8,-5.5,6.67));
#13985=CARTESIAN_POINT('Origin',(-5.8,-5.5,2.2));
#13986=CARTESIAN_POINT('',(-6.075,-5.5,2.2));
#13987=CARTESIAN_POINT('Origin',(-5.8,-5.5,2.2));
#13988=CARTESIAN_POINT('Origin',(-5.8,-8.5,2.2));
#13989=CARTESIAN_POINT('',(-6.3,-8.5,2.2));
#13990=CARTESIAN_POINT('Origin',(-5.8,-8.5,2.2));
#13991=CARTESIAN_POINT('',(-6.3,-8.5,6.67));
#13992=CARTESIAN_POINT('',(-6.3,-8.5,2.2));
#13993=CARTESIAN_POINT('Origin',(-5.8,-8.5,6.67));
#13994=CARTESIAN_POINT('Origin',(-5.8,-8.5,2.2));
#13995=CARTESIAN_POINT('',(-6.075,-8.5,2.2));
#13996=CARTESIAN_POINT('Origin',(-5.8,-8.5,2.2));
#13997=CARTESIAN_POINT('Origin',(5.8,-5.5,2.2));
#13998=CARTESIAN_POINT('',(5.3,-5.5,2.2));
#13999=CARTESIAN_POINT('Origin',(5.8,-5.5,2.2));
#14000=CARTESIAN_POINT('',(5.3,-5.5,6.67));
#14001=CARTESIAN_POINT('',(5.3,-5.5,2.2));
#14002=CARTESIAN_POINT('Origin',(5.8,-5.5,6.67));
#14003=CARTESIAN_POINT('Origin',(5.8,-5.5,2.2));
#14004=CARTESIAN_POINT('',(5.525,-5.5,2.2));
#14005=CARTESIAN_POINT('Origin',(5.8,-5.5,2.2));
#14006=CARTESIAN_POINT('Origin',(5.8,-8.5,0.9));
#14007=CARTESIAN_POINT('',(5.525,-8.5,1.));
#14008=CARTESIAN_POINT('Origin',(5.8,-8.5,1.));
#14009=CARTESIAN_POINT('',(5.525,-8.5,0.9));
#14010=CARTESIAN_POINT('Origin',(-5.8,-5.5,0.9));
#14011=CARTESIAN_POINT('',(-6.075,-5.5,1.));
#14012=CARTESIAN_POINT('Origin',(-5.8,-5.5,1.));
#14013=CARTESIAN_POINT('',(-6.075,-5.5,0.9));
#14014=CARTESIAN_POINT('Origin',(-5.8,-8.5,0.9));
#14015=CARTESIAN_POINT('',(-6.075,-8.5,1.));
#14016=CARTESIAN_POINT('Origin',(-5.8,-8.5,1.));
#14017=CARTESIAN_POINT('',(-6.075,-8.5,0.9));
#14018=CARTESIAN_POINT('Origin',(5.8,-5.5,0.9));
#14019=CARTESIAN_POINT('',(5.525,-5.5,1.));
#14020=CARTESIAN_POINT('Origin',(5.8,-5.5,1.));
#14021=CARTESIAN_POINT('',(5.525,-5.5,0.9));
#14022=CARTESIAN_POINT('Origin',(7.,-4.75,1.));
#14023=CARTESIAN_POINT('',(7.,-4.75,1.));
#14024=CARTESIAN_POINT('',(-7.,-4.75,1.));
#14025=CARTESIAN_POINT('',(7.,-4.75,1.));
#14026=CARTESIAN_POINT('',(-7.,-4.75,6.67));
#14027=CARTESIAN_POINT('',(-7.,-4.75,1.));
#14028=CARTESIAN_POINT('',(7.,-4.75,6.67));
#14029=CARTESIAN_POINT('',(7.,-4.75,6.67));
#14030=CARTESIAN_POINT('',(7.,-4.75,1.));
#14031=CARTESIAN_POINT('Origin',(7.,-9.25,1.));
#14032=CARTESIAN_POINT('',(7.,-9.25,1.));
#14033=CARTESIAN_POINT('',(7.,-9.25,1.));
#14034=CARTESIAN_POINT('',(7.,-9.25,6.67));
#14035=CARTESIAN_POINT('',(7.,-9.25,6.67));
#14036=CARTESIAN_POINT('',(7.,-9.25,1.));
#14037=CARTESIAN_POINT('Origin',(-7.,-9.25,1.));
#14038=CARTESIAN_POINT('',(-7.,-9.25,1.));
#14039=CARTESIAN_POINT('',(-7.,-9.25,1.));
#14040=CARTESIAN_POINT('',(-7.,-9.25,6.67));
#14041=CARTESIAN_POINT('',(-7.,-9.25,6.67));
#14042=CARTESIAN_POINT('',(-7.,-9.25,1.));
#14043=CARTESIAN_POINT('Origin',(-7.,-4.75,1.));
#14044=CARTESIAN_POINT('',(-7.,-4.75,1.));
#14045=CARTESIAN_POINT('',(-7.,-4.75,6.67));
#14046=CARTESIAN_POINT('Origin',(0.,-7.,6.67));
#14047=CARTESIAN_POINT('Origin',(0.,-7.,1.));
#14048=CARTESIAN_POINT('',(0.,0.,0.));
#14049=CARTESIAN_POINT('Origin',(-4.75,-7.,6.67));
#14050=CARTESIAN_POINT('',(-5.175,-7.,7.87));
#14051=CARTESIAN_POINT('Origin',(-4.75,-7.,7.87));
#14052=CARTESIAN_POINT('',(-5.175,-7.,6.67));
#14053=CARTESIAN_POINT('',(-5.175,-7.,6.67));
#14054=CARTESIAN_POINT('Origin',(-4.75,-7.,6.67));
#14055=CARTESIAN_POINT('Origin',(-4.75,-7.,6.67));
#14056=CARTESIAN_POINT('',(-5.395,-7.,7.87));
#14057=CARTESIAN_POINT('Origin',(-4.75,-7.,7.87));
#14058=CARTESIAN_POINT('',(-5.395,-7.,6.67));
#14059=CARTESIAN_POINT('',(-5.395,-7.,6.67));
#14060=CARTESIAN_POINT('Origin',(-4.75,-7.,6.67));
#14061=CARTESIAN_POINT('Origin',(-4.75,-7.,7.87));
#14062=CARTESIAN_POINT('Origin',(-4.75,-7.,6.67));
#14063=CARTESIAN_POINT('',(0.,0.,0.));
#14064=CARTESIAN_POINT('Origin',(4.75,-7.,6.67));
#14065=CARTESIAN_POINT('',(4.325,-7.,7.87));
#14066=CARTESIAN_POINT('Origin',(4.75,-7.,7.87));
#14067=CARTESIAN_POINT('',(4.325,-7.,6.67));
#14068=CARTESIAN_POINT('',(4.325,-7.,6.67));
#14069=CARTESIAN_POINT('Origin',(4.75,-7.,6.67));
#14070=CARTESIAN_POINT('Origin',(4.75,-7.,6.67));
#14071=CARTESIAN_POINT('',(4.105,-7.,7.87));
#14072=CARTESIAN_POINT('Origin',(4.75,-7.,7.87));
#14073=CARTESIAN_POINT('',(4.105,-7.,6.67));
#14074=CARTESIAN_POINT('',(4.105,-7.,6.67));
#14075=CARTESIAN_POINT('Origin',(4.75,-7.,6.67));
#14076=CARTESIAN_POINT('Origin',(4.75,-7.,7.87));
#14077=CARTESIAN_POINT('Origin',(4.75,-7.,6.67));
#14078=CARTESIAN_POINT('',(0.,0.,0.));
#14079=CARTESIAN_POINT('Origin',(4.8,0.,1.6));
#14080=CARTESIAN_POINT('',(4.4,-4.89858719658942E-17,1.6));
#14081=CARTESIAN_POINT('',(4.4,-4.89858719658942E-17,2.7));
#14082=CARTESIAN_POINT('',(4.4,-4.89858719658942E-17,1.6));
#14083=CARTESIAN_POINT('',(5.2,0.,1.6));
#14084=CARTESIAN_POINT('Origin',(4.8,0.,1.6));
#14085=CARTESIAN_POINT('',(5.2,0.,2.7));
#14086=CARTESIAN_POINT('',(5.2,0.,1.6));
#14087=CARTESIAN_POINT('Origin',(4.8,0.,2.7));
#14088=CARTESIAN_POINT('Origin',(3.2,0.,1.6));
#14089=CARTESIAN_POINT('',(2.8,-4.89858719658941E-17,1.6));
#14090=CARTESIAN_POINT('Origin',(3.2,0.,1.6));
#14091=CARTESIAN_POINT('',(2.8,0.,2.7));
#14092=CARTESIAN_POINT('',(2.8,0.,1.6));
#14093=CARTESIAN_POINT('Origin',(3.2,0.,2.7));
#14094=CARTESIAN_POINT('',(2.8,0.,1.6));
#14095=CARTESIAN_POINT('Origin',(3.2,0.,1.6));
#14096=CARTESIAN_POINT('',(2.975,-2.75545529808155E-17,1.6));
#14097=CARTESIAN_POINT('Origin',(3.2,0.,1.6));
#14098=CARTESIAN_POINT('Origin',(4.8,0.,1.6));
#14099=CARTESIAN_POINT('Origin',(4.8,0.,2.7));
#14100=CARTESIAN_POINT('',(5.2,0.,1.6));
#14101=CARTESIAN_POINT('Origin',(4.8,0.,1.6));
#14102=CARTESIAN_POINT('Origin',(4.8,0.,1.6));
#14103=CARTESIAN_POINT('',(4.575,-2.75545529808154E-17,1.6));
#14104=CARTESIAN_POINT('Origin',(4.8,0.,1.6));
#14105=CARTESIAN_POINT('Origin',(4.,0.,2.7));
#14106=CARTESIAN_POINT('',(2.8,4.6,2.7));
#14107=CARTESIAN_POINT('',(2.8,4.6,2.7));
#14108=CARTESIAN_POINT('',(2.8,-4.6,2.7));
#14109=CARTESIAN_POINT('',(2.8,4.6,2.7));
#14110=CARTESIAN_POINT('',(5.2,-4.6,2.7));
#14111=CARTESIAN_POINT('',(2.8,-4.6,2.7));
#14112=CARTESIAN_POINT('',(5.2,-4.6,2.7));
#14113=CARTESIAN_POINT('',(5.2,4.6,2.7));
#14114=CARTESIAN_POINT('',(5.2,-4.6,2.7));
#14115=CARTESIAN_POINT('',(5.2,4.6,2.7));
#14116=CARTESIAN_POINT('',(3.79,4.1,2.7));
#14117=CARTESIAN_POINT('Origin',(4.,4.1,2.7));
#14118=CARTESIAN_POINT('',(3.79,-4.1,2.7));
#14119=CARTESIAN_POINT('Origin',(4.,-4.1,2.7));
#14120=CARTESIAN_POINT('',(3.79,-0.9,2.7));
#14121=CARTESIAN_POINT('Origin',(4.,-0.9,2.7));
#14122=CARTESIAN_POINT('',(3.79,0.9,2.7));
#14123=CARTESIAN_POINT('Origin',(4.,0.9,2.7));
#14124=CARTESIAN_POINT('Origin',(3.2,0.,0.9));
#14125=CARTESIAN_POINT('',(2.975,-2.75545529808155E-17,1.));
#14126=CARTESIAN_POINT('Origin',(3.2,0.,1.));
#14127=CARTESIAN_POINT('',(2.975,-2.75545529808155E-17,0.9));
#14128=CARTESIAN_POINT('Origin',(4.8,0.,0.9));
#14129=CARTESIAN_POINT('',(4.575,-2.75545529808154E-17,1.));
#14130=CARTESIAN_POINT('Origin',(4.8,0.,1.));
#14131=CARTESIAN_POINT('',(4.575,-2.75545529808154E-17,0.9));
#14132=CARTESIAN_POINT('Origin',(4.,0.9,1.6));
#14133=CARTESIAN_POINT('',(3.79,0.9,1.6));
#14134=CARTESIAN_POINT('Origin',(4.,0.9,1.6));
#14135=CARTESIAN_POINT('',(3.79,0.9,1.6));
#14136=CARTESIAN_POINT('Origin',(4.,0.9,1.6));
#14137=CARTESIAN_POINT('Origin',(4.,-0.9,1.6));
#14138=CARTESIAN_POINT('',(3.79,-0.9,1.6));
#14139=CARTESIAN_POINT('Origin',(4.,-0.9,1.6));
#14140=CARTESIAN_POINT('',(3.79,-0.9,1.6));
#14141=CARTESIAN_POINT('Origin',(4.,-0.9,1.6));
#14142=CARTESIAN_POINT('Origin',(4.,-4.1,1.6));
#14143=CARTESIAN_POINT('',(3.79,-4.1,1.6));
#14144=CARTESIAN_POINT('Origin',(4.,-4.1,1.6));
#14145=CARTESIAN_POINT('',(3.79,-4.1,1.6));
#14146=CARTESIAN_POINT('Origin',(4.,-4.1,1.6));
#14147=CARTESIAN_POINT('Origin',(4.,4.1,1.6));
#14148=CARTESIAN_POINT('',(3.79,4.1,1.6));
#14149=CARTESIAN_POINT('Origin',(4.,4.1,1.6));
#14150=CARTESIAN_POINT('',(3.79,4.1,1.6));
#14151=CARTESIAN_POINT('Origin',(4.,4.1,1.6));
#14152=CARTESIAN_POINT('Origin',(5.2,4.6,1.));
#14153=CARTESIAN_POINT('',(5.2,4.6,1.));
#14154=CARTESIAN_POINT('',(2.8,4.6,1.));
#14155=CARTESIAN_POINT('',(5.2,4.6,1.));
#14156=CARTESIAN_POINT('',(2.8,4.6,1.));
#14157=CARTESIAN_POINT('',(5.2,4.6,1.));
#14158=CARTESIAN_POINT('Origin',(5.2,-4.6,1.));
#14159=CARTESIAN_POINT('',(5.2,-4.6,1.));
#14160=CARTESIAN_POINT('',(5.2,-4.6,1.));
#14161=CARTESIAN_POINT('',(5.2,-4.6,1.));
#14162=CARTESIAN_POINT('Origin',(2.8,-4.6,1.));
#14163=CARTESIAN_POINT('',(2.8,-4.6,1.));
#14164=CARTESIAN_POINT('',(2.8,-4.6,1.));
#14165=CARTESIAN_POINT('',(2.8,-4.6,1.));
#14166=CARTESIAN_POINT('Origin',(2.8,4.6,1.));
#14167=CARTESIAN_POINT('',(2.8,4.6,1.));
#14168=CARTESIAN_POINT('Origin',(4.,0.,1.));
#14169=CARTESIAN_POINT('',(0.,0.,0.));
#14170=CARTESIAN_POINT('Origin',(20.8,0.,1.6));
#14171=CARTESIAN_POINT('',(20.4,-4.8985871965894E-17,1.6));
#14172=CARTESIAN_POINT('',(20.4,-4.8985871965894E-17,2.7));
#14173=CARTESIAN_POINT('',(20.4,-4.8985871965894E-17,1.6));
#14174=CARTESIAN_POINT('',(21.2,0.,1.6));
#14175=CARTESIAN_POINT('Origin',(20.8,0.,1.6));
#14176=CARTESIAN_POINT('',(21.2,0.,2.7));
#14177=CARTESIAN_POINT('',(21.2,0.,1.6));
#14178=CARTESIAN_POINT('Origin',(20.8,0.,2.7));
#14179=CARTESIAN_POINT('Origin',(19.2,0.,1.6));
#14180=CARTESIAN_POINT('',(18.8,-4.8985871965894E-17,1.6));
#14181=CARTESIAN_POINT('Origin',(19.2,0.,1.6));
#14182=CARTESIAN_POINT('',(18.8,0.,2.7));
#14183=CARTESIAN_POINT('',(18.8,0.,1.6));
#14184=CARTESIAN_POINT('Origin',(19.2,0.,2.7));
#14185=CARTESIAN_POINT('',(18.8,0.,1.6));
#14186=CARTESIAN_POINT('Origin',(19.2,0.,1.6));
#14187=CARTESIAN_POINT('',(18.975,-2.75545529808156E-17,1.6));
#14188=CARTESIAN_POINT('Origin',(19.2,0.,1.6));
#14189=CARTESIAN_POINT('Origin',(20.8,0.,1.6));
#14190=CARTESIAN_POINT('Origin',(20.8,0.,2.7));
#14191=CARTESIAN_POINT('',(21.2,0.,1.6));
#14192=CARTESIAN_POINT('Origin',(20.8,0.,1.6));
#14193=CARTESIAN_POINT('Origin',(20.8,0.,1.6));
#14194=CARTESIAN_POINT('',(20.575,-2.75545529808156E-17,1.6));
#14195=CARTESIAN_POINT('Origin',(20.8,0.,1.6));
#14196=CARTESIAN_POINT('Origin',(20.,0.,2.7));
#14197=CARTESIAN_POINT('',(18.8,4.6,2.7));
#14198=CARTESIAN_POINT('',(18.8,4.6,2.7));
#14199=CARTESIAN_POINT('',(18.8,-4.6,2.7));
#14200=CARTESIAN_POINT('',(18.8,4.6,2.7));
#14201=CARTESIAN_POINT('',(21.2,-4.6,2.7));
#14202=CARTESIAN_POINT('',(18.8,-4.6,2.7));
#14203=CARTESIAN_POINT('',(21.2,-4.6,2.7));
#14204=CARTESIAN_POINT('',(21.2,4.6,2.7));
#14205=CARTESIAN_POINT('',(21.2,-4.6,2.7));
#14206=CARTESIAN_POINT('',(21.2,4.6,2.7));
#14207=CARTESIAN_POINT('',(19.79,4.1,2.7));
#14208=CARTESIAN_POINT('Origin',(20.,4.1,2.7));
#14209=CARTESIAN_POINT('',(19.79,-4.1,2.7));
#14210=CARTESIAN_POINT('Origin',(20.,-4.1,2.7));
#14211=CARTESIAN_POINT('',(19.79,-0.9,2.7));
#14212=CARTESIAN_POINT('Origin',(20.,-0.9,2.7));
#14213=CARTESIAN_POINT('',(19.79,0.9,2.7));
#14214=CARTESIAN_POINT('Origin',(20.,0.9,2.7));
#14215=CARTESIAN_POINT('Origin',(19.2,0.,0.9));
#14216=CARTESIAN_POINT('',(18.975,-2.75545529808156E-17,1.));
#14217=CARTESIAN_POINT('Origin',(19.2,0.,1.));
#14218=CARTESIAN_POINT('',(18.975,-2.75545529808156E-17,0.9));
#14219=CARTESIAN_POINT('Origin',(20.8,0.,0.9));
#14220=CARTESIAN_POINT('',(20.575,-2.75545529808156E-17,1.));
#14221=CARTESIAN_POINT('Origin',(20.8,0.,1.));
#14222=CARTESIAN_POINT('',(20.575,-2.75545529808156E-17,0.9));
#14223=CARTESIAN_POINT('Origin',(20.,0.9,1.6));
#14224=CARTESIAN_POINT('',(19.79,0.9,1.6));
#14225=CARTESIAN_POINT('Origin',(20.,0.9,1.6));
#14226=CARTESIAN_POINT('',(19.79,0.9,1.6));
#14227=CARTESIAN_POINT('Origin',(20.,0.9,1.6));
#14228=CARTESIAN_POINT('Origin',(20.,-0.9,1.6));
#14229=CARTESIAN_POINT('',(19.79,-0.9,1.6));
#14230=CARTESIAN_POINT('Origin',(20.,-0.9,1.6));
#14231=CARTESIAN_POINT('',(19.79,-0.9,1.6));
#14232=CARTESIAN_POINT('Origin',(20.,-0.9,1.6));
#14233=CARTESIAN_POINT('Origin',(20.,-4.1,1.6));
#14234=CARTESIAN_POINT('',(19.79,-4.1,1.6));
#14235=CARTESIAN_POINT('Origin',(20.,-4.1,1.6));
#14236=CARTESIAN_POINT('',(19.79,-4.1,1.6));
#14237=CARTESIAN_POINT('Origin',(20.,-4.1,1.6));
#14238=CARTESIAN_POINT('Origin',(20.,4.1,1.6));
#14239=CARTESIAN_POINT('',(19.79,4.1,1.6));
#14240=CARTESIAN_POINT('Origin',(20.,4.1,1.6));
#14241=CARTESIAN_POINT('',(19.79,4.1,1.6));
#14242=CARTESIAN_POINT('Origin',(20.,4.1,1.6));
#14243=CARTESIAN_POINT('Origin',(21.2,4.6,1.));
#14244=CARTESIAN_POINT('',(21.2,4.6,1.));
#14245=CARTESIAN_POINT('',(18.8,4.6,1.));
#14246=CARTESIAN_POINT('',(21.2,4.6,1.));
#14247=CARTESIAN_POINT('',(18.8,4.6,1.));
#14248=CARTESIAN_POINT('',(21.2,4.6,1.));
#14249=CARTESIAN_POINT('Origin',(21.2,-4.6,1.));
#14250=CARTESIAN_POINT('',(21.2,-4.6,1.));
#14251=CARTESIAN_POINT('',(21.2,-4.6,1.));
#14252=CARTESIAN_POINT('',(21.2,-4.6,1.));
#14253=CARTESIAN_POINT('Origin',(18.8,-4.6,1.));
#14254=CARTESIAN_POINT('',(18.8,-4.6,1.));
#14255=CARTESIAN_POINT('',(18.8,-4.6,1.));
#14256=CARTESIAN_POINT('',(18.8,-4.6,1.));
#14257=CARTESIAN_POINT('Origin',(18.8,4.6,1.));
#14258=CARTESIAN_POINT('',(18.8,4.6,1.));
#14259=CARTESIAN_POINT('Origin',(20.,0.,1.));
#14260=CARTESIAN_POINT('',(0.,0.,0.));
#14261=CARTESIAN_POINT('Origin',(-6.,9.,-0.5));
#14262=CARTESIAN_POINT('',(-6.,9.,-0.5));
#14263=CARTESIAN_POINT('',(-8.,9.,-0.5));
#14264=CARTESIAN_POINT('',(-6.,9.,-0.5));
#14265=CARTESIAN_POINT('',(-8.,9.,0.));
#14266=CARTESIAN_POINT('',(-8.,9.,-0.5));
#14267=CARTESIAN_POINT('',(-6.,9.,0.));
#14268=CARTESIAN_POINT('',(-6.,9.,0.));
#14269=CARTESIAN_POINT('',(-6.,9.,-0.5));
#14270=CARTESIAN_POINT('Origin',(-6.,-18.,-0.5));
#14271=CARTESIAN_POINT('',(-6.,-18.,-0.5));
#14272=CARTESIAN_POINT('',(-6.,-18.,-0.5));
#14273=CARTESIAN_POINT('',(-6.,-18.,0.));
#14274=CARTESIAN_POINT('',(-6.,-18.,0.));
#14275=CARTESIAN_POINT('',(-6.,-18.,-0.5));
#14276=CARTESIAN_POINT('Origin',(-8.,-18.,-0.5));
#14277=CARTESIAN_POINT('',(-8.,-18.,-0.5));
#14278=CARTESIAN_POINT('',(-8.,-18.,-0.5));
#14279=CARTESIAN_POINT('',(-8.,-18.,0.));
#14280=CARTESIAN_POINT('',(-8.,-18.,0.));
#14281=CARTESIAN_POINT('',(-8.,-18.,-0.5));
#14282=CARTESIAN_POINT('Origin',(-8.,9.,-0.5));
#14283=CARTESIAN_POINT('',(-8.,9.,-0.5));
#14284=CARTESIAN_POINT('',(-8.,9.,0.));
#14285=CARTESIAN_POINT('Origin',(-7.,-4.5,0.));
#14286=CARTESIAN_POINT('Origin',(-7.,-4.5,-0.5));
#14287=CARTESIAN_POINT('',(0.,0.,0.));
#14288=CARTESIAN_POINT('Origin',(24.,9.,-0.5));
#14289=CARTESIAN_POINT('',(24.,9.,-0.5));
#14290=CARTESIAN_POINT('',(22.,9.,-0.5));
#14291=CARTESIAN_POINT('',(24.,9.,-0.5));
#14292=CARTESIAN_POINT('',(22.,9.,0.));
#14293=CARTESIAN_POINT('',(22.,9.,-0.5));
#14294=CARTESIAN_POINT('',(24.,9.,0.));
#14295=CARTESIAN_POINT('',(24.,9.,0.));
#14296=CARTESIAN_POINT('',(24.,9.,-0.5));
#14297=CARTESIAN_POINT('Origin',(24.,-18.,-0.5));
#14298=CARTESIAN_POINT('',(24.,-18.,-0.5));
#14299=CARTESIAN_POINT('',(24.,-18.,-0.5));
#14300=CARTESIAN_POINT('',(24.,-18.,0.));
#14301=CARTESIAN_POINT('',(24.,-18.,0.));
#14302=CARTESIAN_POINT('',(24.,-18.,-0.5));
#14303=CARTESIAN_POINT('Origin',(22.,-18.,-0.5));
#14304=CARTESIAN_POINT('',(22.,-18.,-0.5));
#14305=CARTESIAN_POINT('',(22.,-18.,-0.5));
#14306=CARTESIAN_POINT('',(22.,-18.,0.));
#14307=CARTESIAN_POINT('',(22.,-18.,0.));
#14308=CARTESIAN_POINT('',(22.,-18.,-0.5));
#14309=CARTESIAN_POINT('Origin',(22.,9.,-0.5));
#14310=CARTESIAN_POINT('',(22.,9.,-0.5));
#14311=CARTESIAN_POINT('',(22.,9.,0.));
#14312=CARTESIAN_POINT('Origin',(23.,-4.5,0.));
#14313=CARTESIAN_POINT('Origin',(23.,-4.5,-0.5));
#14314=CARTESIAN_POINT('',(0.,0.,0.));
#14315=CARTESIAN_POINT('Origin',(0.375,0.5,0.));
#14316=CARTESIAN_POINT('',(-0.375,0.5,-4.59242549680257E-17));
#14317=CARTESIAN_POINT('Origin',(0.,0.5,0.));
#14318=CARTESIAN_POINT('Origin',(0.,0.475,0.));
#14319=CARTESIAN_POINT('',(-0.425,0.45,-5.20474889637625E-17));
#14320=CARTESIAN_POINT('Origin',(0.,0.45,0.));
#14321=CARTESIAN_POINT('',(-0.4,0.475,-4.89858719658941E-17));
#14322=CARTESIAN_POINT('Origin',(0.,0.24,0.));
#14323=CARTESIAN_POINT('',(-0.425,0.0299999999999998,-5.20474889637625E-17));
#14324=CARTESIAN_POINT('Origin',(0.,0.0299999999999998,0.));
#14325=CARTESIAN_POINT('',(-0.425,0.24,-5.20474889637625E-17));
#14326=CARTESIAN_POINT('Origin',(0.,0.0150000000000001,0.));
#14327=CARTESIAN_POINT('',(-0.395,4.85722573273506E-17,-4.83735485663204E-17));
#14328=CARTESIAN_POINT('Origin',(0.,0.,0.));
#14329=CARTESIAN_POINT('',(-0.41,0.0150000000000001,-5.02105187650415E-17));
#14330=CARTESIAN_POINT('Origin',(0.27,0.,0.));
#14331=CARTESIAN_POINT('',(-0.27,0.,-3.30654635769785E-17));
#14332=CARTESIAN_POINT('Origin',(0.,0.,0.));
#14333=CARTESIAN_POINT('Origin',(0.,-0.02,0.));
#14334=CARTESIAN_POINT('',(-0.24505,-0.0498999999999999,3.00099698131059E-17));
#14335=CARTESIAN_POINT('Origin',(0.,-0.0498999999999999,0.));
#14336=CARTESIAN_POINT('',(-0.26,-0.02,-3.18408167778312E-17));
#14337=CARTESIAN_POINT('Origin',(0.,-0.995,0.));
#14338=CARTESIAN_POINT('',(-0.24505,-1.95495,3.00099698131059E-17));
#14339=CARTESIAN_POINT('Origin',(0.,-1.95495,0.));
#14340=CARTESIAN_POINT('',(-0.24505,-0.995,-3.00099698131059E-17));
#14341=CARTESIAN_POINT('Origin',(0.,-1.975,0.));
#14342=CARTESIAN_POINT('',(-0.2,-2.,-2.44929359829471E-17));
#14343=CARTESIAN_POINT('Origin',(0.,-2.,0.));
#14344=CARTESIAN_POINT('',(-0.225,-1.975,-2.75545529808154E-17));
#14345=CARTESIAN_POINT('Origin',(0.,-2.,0.));
#14346=CARTESIAN_POINT('Origin',(0.115470053837925,-0.5,-0.2));
#14347=CARTESIAN_POINT('',(0.23094010767585,-0.5,0.));
#14348=CARTESIAN_POINT('',(0.115470053837925,-0.5,-0.2));
#14349=CARTESIAN_POINT('',(0.23094010767585,-0.5,0.));
#14350=CARTESIAN_POINT('',(0.115470053837925,-0.8,-0.2));
#14351=CARTESIAN_POINT('',(0.115470053837925,-0.5,-0.2));
#14352=CARTESIAN_POINT('',(0.23094010767585,-0.8,0.));
#14353=CARTESIAN_POINT('',(0.23094010767585,-0.8,0.));
#14354=CARTESIAN_POINT('',(0.23094010767585,-0.5,0.));
#14355=CARTESIAN_POINT('Origin',(-0.115470053837925,-0.5,-0.2));
#14356=CARTESIAN_POINT('',(-0.115470053837925,-0.5,-0.2));
#14357=CARTESIAN_POINT('',(0.115470053837925,-0.5,-0.2));
#14358=CARTESIAN_POINT('',(-0.115470053837925,-0.8,-0.2));
#14359=CARTESIAN_POINT('',(-0.115470053837925,-0.5,-0.2));
#14360=CARTESIAN_POINT('',(0.115470053837925,-0.8,-0.2));
#14361=CARTESIAN_POINT('Origin',(-0.23094010767585,-0.5,-2.77555756156289E-17));
#14362=CARTESIAN_POINT('',(-0.23094010767585,-0.5,-2.82820063659975E-17));
#14363=CARTESIAN_POINT('',(-0.115470053837925,-0.5,-0.2));
#14364=CARTESIAN_POINT('',(-0.23094010767585,-0.8,-2.77555756156289E-17));
#14365=CARTESIAN_POINT('',(-0.23094010767585,-0.5,-2.82820063659975E-17));
#14366=CARTESIAN_POINT('',(-0.115470053837925,-0.8,-0.2));
#14367=CARTESIAN_POINT('Origin',(-0.115470053837925,-0.5,0.2));
#14368=CARTESIAN_POINT('',(-0.115470053837925,-0.5,0.2));
#14369=CARTESIAN_POINT('',(-0.23094010767585,-0.5,-2.82820063659975E-17));
#14370=CARTESIAN_POINT('',(-0.115470053837925,-0.8,0.2));
#14371=CARTESIAN_POINT('',(-0.115470053837925,-0.5,0.2));
#14372=CARTESIAN_POINT('',(-0.23094010767585,-0.8,-2.82820063659975E-17));
#14373=CARTESIAN_POINT('Origin',(0.115470053837925,-0.5,0.2));
#14374=CARTESIAN_POINT('',(0.115470053837925,-0.5,0.2));
#14375=CARTESIAN_POINT('',(-0.115470053837925,-0.5,0.2));
#14376=CARTESIAN_POINT('',(0.115470053837925,-0.8,0.2));
#14377=CARTESIAN_POINT('',(0.115470053837925,-0.5,0.2));
#14378=CARTESIAN_POINT('',(-0.115470053837925,-0.8,0.2));
#14379=CARTESIAN_POINT('Origin',(0.23094010767585,-0.5,0.));
#14380=CARTESIAN_POINT('',(0.115470053837925,-0.5,0.2));
#14381=CARTESIAN_POINT('',(0.115470053837925,-0.8,0.2));
#14382=CARTESIAN_POINT('Origin',(0.,-0.5,0.));
#14383=CARTESIAN_POINT('Origin',(0.,-0.8,0.));
#14384=CARTESIAN_POINT('',(0.,0.,0.));
#14385=CARTESIAN_POINT('',(0.,0.,0.));
#14386=CARTESIAN_POINT('Origin',(0.,0.,0.));
#14387=CARTESIAN_POINT('',(-2.05,-1.65,2.51052593825207E-16));
#14388=CARTESIAN_POINT('Origin',(0.,-1.65,0.));
#14389=CARTESIAN_POINT('',(-2.05,-1.14891252930761,-2.51052593825207E-16));
#14390=CARTESIAN_POINT('',(-2.05,0.,2.51052593825207E-16));
#14391=CARTESIAN_POINT('Origin',(0.,-1.14891252930761,0.));
#14392=CARTESIAN_POINT('Origin',(0.,0.,0.));
#14393=CARTESIAN_POINT('',(-2.05,1.14891252930761,2.51052593825207E-16));
#14394=CARTESIAN_POINT('Origin',(0.,1.14891252930761,0.));
#14395=CARTESIAN_POINT('',(-2.05,1.65,-2.51052593825207E-16));
#14396=CARTESIAN_POINT('',(-2.05,0.,2.51052593825207E-16));
#14397=CARTESIAN_POINT('Origin',(0.,1.65,0.));
#14398=CARTESIAN_POINT('Origin',(0.,0.,0.));
#14399=CARTESIAN_POINT('',(-1.43895998899814E-16,-1.76221774462768E-32,
-2.35));
#14400=CARTESIAN_POINT('',(-1.43895998899814E-16,-1.76221774462768E-32,
2.35));
#14401=CARTESIAN_POINT('Origin',(0.,0.,0.));
#14402=CARTESIAN_POINT('Origin',(0.,1.55,-1.49));
#14403=CARTESIAN_POINT('',(-3.76384615384615,1.55,-2.13));
#14404=CARTESIAN_POINT('',(-1.81744325908679,1.55,-2.13));
#14405=CARTESIAN_POINT('',(0.,1.55,-2.13));
#14406=CARTESIAN_POINT('',(-2.46585583768694,1.55,-1.32648218523477));
#14407=CARTESIAN_POINT('',(-1.68,1.55,-0.84));
#14408=CARTESIAN_POINT('Origin',(0.,1.55,0.));
#14409=CARTESIAN_POINT('Origin',(0.,1.55,-1.49));
#14410=CARTESIAN_POINT('',(1.81744325908679,1.55,-2.13));
#14411=CARTESIAN_POINT('',(3.76384615384615,1.55,-2.13));
#14412=CARTESIAN_POINT('',(0.,1.55,-2.13));
#14413=CARTESIAN_POINT('',(2.46585583768694,1.55,-1.32648218523477));
#14414=CARTESIAN_POINT('Origin',(0.,1.55,0.));
#14415=CARTESIAN_POINT('',(3.78,1.55,-2.14));
#14416=CARTESIAN_POINT('Origin',(0.,-1.55,-1.49));
#14417=CARTESIAN_POINT('',(-1.81744325908679,-1.55,-2.13));
#14418=CARTESIAN_POINT('',(-3.76384615384615,-1.55,-2.13));
#14419=CARTESIAN_POINT('',(0.,-1.55,-2.13));
#14420=CARTESIAN_POINT('',(-2.46585583768694,-1.55,-1.32648218523477));
#14421=CARTESIAN_POINT('Origin',(0.,-1.55,0.));
#14422=CARTESIAN_POINT('',(-1.68,-1.55,-0.84));
#14423=CARTESIAN_POINT('Origin',(-3.78,0.,-2.14));
#14424=CARTESIAN_POINT('',(-3.76384615384615,0.,-2.13));
#14425=CARTESIAN_POINT('',(-2.46585583768694,0.,-1.32648218523477));
#14426=CARTESIAN_POINT('Origin',(0.,-1.55,-1.49));
#14427=CARTESIAN_POINT('',(3.76384615384615,-1.55,-2.13));
#14428=CARTESIAN_POINT('',(1.81744325908679,-1.55,-2.13));
#14429=CARTESIAN_POINT('',(0.,-1.55,-2.13));
#14430=CARTESIAN_POINT('',(2.46585583768694,-1.55,-1.32648218523477));
#14431=CARTESIAN_POINT('',(3.78,-1.55,-2.14));
#14432=CARTESIAN_POINT('Origin',(0.,-1.55,0.));
#14433=CARTESIAN_POINT('Origin',(1.68,0.,-0.84));
#14434=CARTESIAN_POINT('',(3.76384615384615,0.,-2.13));
#14435=CARTESIAN_POINT('',(2.46585583768694,0.,-1.32648218523477));
#14436=CARTESIAN_POINT('Origin',(0.,0.,-2.13));
#14437=CARTESIAN_POINT('',(-6.35,1.9,-2.13));
#14438=CARTESIAN_POINT('',(-6.35,-1.9,-2.13));
#14439=CARTESIAN_POINT('',(-6.35,1.9,-2.13));
#14440=CARTESIAN_POINT('',(6.35,-1.9,-2.13));
#14441=CARTESIAN_POINT('',(-6.35,-1.9,-2.13));
#14442=CARTESIAN_POINT('',(6.35,1.9,-2.13));
#14443=CARTESIAN_POINT('',(6.35,-1.9,-2.13));
#14444=CARTESIAN_POINT('',(6.35,1.9,-2.13));
#14445=CARTESIAN_POINT('',(4.1,7.9602041944578E-17,-2.13));
#14446=CARTESIAN_POINT('Origin',(4.75,0.,-2.13));
#14447=CARTESIAN_POINT('',(-5.4,7.9602041944578E-17,-2.13));
#14448=CARTESIAN_POINT('Origin',(-4.75,0.,-2.13));
#14449=CARTESIAN_POINT('',(1.81744325908679,-1.65,-2.13));
#14450=CARTESIAN_POINT('',(1.81744325908679,0.,-2.13));
#14451=CARTESIAN_POINT('',(-1.81744325908679,-1.65,-2.13));
#14452=CARTESIAN_POINT('',(0.,-1.65,-2.13));
#14453=CARTESIAN_POINT('',(-1.81744325908679,0.,-2.13));
#14454=CARTESIAN_POINT('',(-1.81744325908679,1.65,-2.13));
#14455=CARTESIAN_POINT('',(-1.81744325908679,0.,-2.13));
#14456=CARTESIAN_POINT('',(1.81744325908679,1.65,-2.13));
#14457=CARTESIAN_POINT('',(0.,1.65,-2.13));
#14458=CARTESIAN_POINT('',(1.81744325908679,0.,-2.13));
#14459=CARTESIAN_POINT('Origin',(0.,0.,0.));
#14460=CARTESIAN_POINT('Origin',(0.,1.65,0.));
#14461=CARTESIAN_POINT('Origin',(0.,-1.65,0.));
#14462=CARTESIAN_POINT('Origin',(0.,-1.65,0.));
#14463=CARTESIAN_POINT('Origin',(0.,1.65,0.));
#14464=CARTESIAN_POINT('Origin',(3.35,1.4,-3.33));
#14465=CARTESIAN_POINT('',(3.35,1.4,-3.33));
#14466=CARTESIAN_POINT('',(-3.35,1.4,-3.33));
#14467=CARTESIAN_POINT('',(1.675,1.4,-3.33));
#14468=CARTESIAN_POINT('',(3.35,1.4,-2.83));
#14469=CARTESIAN_POINT('',(3.35,1.4,-3.33));
#14470=CARTESIAN_POINT('',(-3.35,1.4,-2.83));
#14471=CARTESIAN_POINT('',(3.35,1.4,-2.83));
#14472=CARTESIAN_POINT('',(-3.35,1.4,-3.33));
#14473=CARTESIAN_POINT('Origin',(3.35,-1.4,-3.33));
#14474=CARTESIAN_POINT('',(3.35,-1.4,-3.33));
#14475=CARTESIAN_POINT('',(3.35,-0.7,-3.33));
#14476=CARTESIAN_POINT('',(3.35,-1.4,-2.83));
#14477=CARTESIAN_POINT('',(3.35,-1.4,-3.33));
#14478=CARTESIAN_POINT('',(3.35,-1.4,-2.83));
#14479=CARTESIAN_POINT('Origin',(-3.35,-1.4,-3.33));
#14480=CARTESIAN_POINT('',(-3.35,-1.4,-3.33));
#14481=CARTESIAN_POINT('',(-1.675,-1.4,-3.33));
#14482=CARTESIAN_POINT('',(-3.35,-1.4,-2.83));
#14483=CARTESIAN_POINT('',(-3.35,-1.4,-3.33));
#14484=CARTESIAN_POINT('',(-3.35,-1.4,-2.83));
#14485=CARTESIAN_POINT('Origin',(-3.35,1.4,-3.33));
#14486=CARTESIAN_POINT('',(-3.35,0.7,-3.33));
#14487=CARTESIAN_POINT('',(-3.35,1.4,-2.83));
#14488=CARTESIAN_POINT('Origin',(0.,0.,-2.83));
#14489=CARTESIAN_POINT('Origin',(-4.75,0.,-3.33));
#14490=CARTESIAN_POINT('',(-5.4,-7.9602041944578E-17,-3.33));
#14491=CARTESIAN_POINT('Origin',(-4.75,0.,-3.33));
#14492=CARTESIAN_POINT('',(-5.4,-7.9602041944578E-17,-3.33));
#14493=CARTESIAN_POINT('Origin',(4.75,0.,-3.33));
#14494=CARTESIAN_POINT('',(4.1,-7.9602041944578E-17,-3.33));
#14495=CARTESIAN_POINT('Origin',(4.75,0.,-3.33));
#14496=CARTESIAN_POINT('',(4.1,-7.9602041944578E-17,-3.33));
#14497=CARTESIAN_POINT('Origin',(6.35,1.9,-3.33));
#14498=CARTESIAN_POINT('',(6.35,1.9,-3.33));
#14499=CARTESIAN_POINT('',(-6.35,1.9,-3.33));
#14500=CARTESIAN_POINT('',(6.35,1.9,-3.33));
#14501=CARTESIAN_POINT('',(-6.35,1.9,-3.33));
#14502=CARTESIAN_POINT('',(6.35,1.9,-3.33));
#14503=CARTESIAN_POINT('Origin',(6.35,-1.9,-3.33));
#14504=CARTESIAN_POINT('',(6.35,-1.9,-3.33));
#14505=CARTESIAN_POINT('',(6.35,-1.9,-3.33));
#14506=CARTESIAN_POINT('',(6.35,-1.9,-3.33));
#14507=CARTESIAN_POINT('Origin',(-6.35,-1.9,-3.33));
#14508=CARTESIAN_POINT('',(-6.35,-1.9,-3.33));
#14509=CARTESIAN_POINT('',(-6.35,-1.9,-3.33));
#14510=CARTESIAN_POINT('',(-6.35,-1.9,-3.33));
#14511=CARTESIAN_POINT('Origin',(-6.35,1.9,-3.33));
#14512=CARTESIAN_POINT('',(-6.35,1.9,-3.33));
#14513=CARTESIAN_POINT('Origin',(0.,0.,-3.33));
#14514=CARTESIAN_POINT('',(0.,0.,0.));
#14515=CARTESIAN_POINT('Origin',(0.,0.,0.));
#14516=CARTESIAN_POINT('',(-1.8,-0.85,-2.20436423846524E-16));
#14517=CARTESIAN_POINT('Origin',(0.,-0.85,0.));
#14518=CARTESIAN_POINT('',(-1.8,0.85,-2.20436423846524E-16));
#14519=CARTESIAN_POINT('',(-1.8,0.,-2.20436423846524E-16));
#14520=CARTESIAN_POINT('Origin',(0.,0.85,0.));
#14521=CARTESIAN_POINT('Origin',(2.19089023002066,0.85,0.));
#14522=CARTESIAN_POINT('',(2.19089023002066,0.85,0.));
#14523=CARTESIAN_POINT('Origin',(0.,0.85,0.));
#14524=CARTESIAN_POINT('Origin',(3.99680288865056E-15,0.,0.));
#14525=CARTESIAN_POINT('',(3.85290688975075E-15,-1.76221774462768E-32,2.35));
#14526=CARTESIAN_POINT('',(3.85290688975075E-15,-1.76221774462768E-32,-2.35));
#14527=CARTESIAN_POINT('Origin',(3.99680288865056E-15,0.,0.));
#14528=CARTESIAN_POINT('',(2.19089023002066,-0.85,0.));
#14529=CARTESIAN_POINT('Origin',(0.,-0.85,0.));
#14530=CARTESIAN_POINT('Origin',(1.8,-0.85,0.));
#14531=CARTESIAN_POINT('Origin',(0.,1.55,0.));
#14532=CARTESIAN_POINT('',(1.42894191624432,1.8,0.825000000000001));
#14533=CARTESIAN_POINT('',(1.53744468918255,1.55,0.598968970568896));
#14534=CARTESIAN_POINT('Ctrl Pts',(1.42894191624432,1.8,0.825000000000001));
#14535=CARTESIAN_POINT('Ctrl Pts',(1.44466308895875,1.8,0.797770130104052));
#14536=CARTESIAN_POINT('Ctrl Pts',(1.46055812562105,1.79370633789704,0.768258557763732));
#14537=CARTESIAN_POINT('Ctrl Pts',(1.48824888379079,1.76817777258318,0.713138492740816));
#14538=CARTESIAN_POINT('Ctrl Pts',(1.50008999307766,1.74894552961493,0.687551581002689));
#14539=CARTESIAN_POINT('Ctrl Pts',(1.51812136280714,1.70460745840382,0.646764802471699));
#14540=CARTESIAN_POINT('Ctrl Pts',(1.52552758004446,1.67652816181843,0.628833667319578));
#14541=CARTESIAN_POINT('Ctrl Pts',(1.53516661651472,1.61494799959182,0.604921184808251));
#14542=CARTESIAN_POINT('Ctrl Pts',(1.53744468918255,1.58144291640553,0.598968970568896));
#14543=CARTESIAN_POINT('Ctrl Pts',(1.53744468918255,1.55,0.598968970568896));
#14544=CARTESIAN_POINT('',(1.42894191624432,1.3,0.825000000000001));
#14545=CARTESIAN_POINT('Ctrl Pts',(1.42894191624432,1.3,0.825000000000001));
#14546=CARTESIAN_POINT('Ctrl Pts',(1.4132207435299,1.3,0.852229869895949));
#14547=CARTESIAN_POINT('Ctrl Pts',(1.39561049050871,1.30629366210296,0.880751161609749));
#14548=CARTESIAN_POINT('Ctrl Pts',(1.36172049302549,1.33182222741682,0.932292094146256));
#14549=CARTESIAN_POINT('Ctrl Pts',(1.34548213209931,1.35105447038507,0.955340251466734));
#14550=CARTESIAN_POINT('Ctrl Pts',(1.31917543061769,1.39539254159618,0.99134926498299));
#14551=CARTESIAN_POINT('Ctrl Pts',(1.30734972067592,1.42347183818157,1.00672880483252));
#14552=CARTESIAN_POINT('Ctrl Pts',(1.29146042158868,1.48505200040818,1.02703269653942));
#14553=CARTESIAN_POINT('Ctrl Pts',(1.28744468918255,1.51855708359447,1.03198167246111));
#14554=CARTESIAN_POINT('Ctrl Pts',(1.28744468918255,1.58144291640553,1.03198167246111));
#14555=CARTESIAN_POINT('Ctrl Pts',(1.29146042158868,1.61494799959182,1.02703269653942));
#14556=CARTESIAN_POINT('Ctrl Pts',(1.30734972067592,1.67652816181843,1.00672880483252));
#14557=CARTESIAN_POINT('Ctrl Pts',(1.31917543061769,1.70460745840382,0.991349264982991));
#14558=CARTESIAN_POINT('Ctrl Pts',(1.34548213209931,1.74894552961493,0.955340251466735));
#14559=CARTESIAN_POINT('Ctrl Pts',(1.36172049302549,1.76817777258318,0.932292094146256));
#14560=CARTESIAN_POINT('Ctrl Pts',(1.39561049050871,1.79370633789704,0.880751161609749));
#14561=CARTESIAN_POINT('Ctrl Pts',(1.4132207435299,1.8,0.85222986989595));
#14562=CARTESIAN_POINT('Ctrl Pts',(1.42894191624432,1.8,0.825000000000001));
#14563=CARTESIAN_POINT('Ctrl Pts',(1.53744468918255,1.55,0.598968970568896));
#14564=CARTESIAN_POINT('Ctrl Pts',(1.53744468918255,1.51855708359447,0.598968970568896));
#14565=CARTESIAN_POINT('Ctrl Pts',(1.53516661651472,1.48505200040818,0.60492118480825));
#14566=CARTESIAN_POINT('Ctrl Pts',(1.52552758004446,1.42347183818157,0.628833667319578));
#14567=CARTESIAN_POINT('Ctrl Pts',(1.51812136280714,1.39539254159618,0.646764802471699));
#14568=CARTESIAN_POINT('Ctrl Pts',(1.50008999307766,1.35105447038507,0.687551581002689));
#14569=CARTESIAN_POINT('Ctrl Pts',(1.48824888379079,1.33182222741682,0.713138492740816));
#14570=CARTESIAN_POINT('Ctrl Pts',(1.46055812562105,1.30629366210296,0.768258557763732));
#14571=CARTESIAN_POINT('Ctrl Pts',(1.44466308895875,1.3,0.797770130104052));
#14572=CARTESIAN_POINT('Ctrl Pts',(1.42894191624432,1.3,0.825000000000001));
#14573=CARTESIAN_POINT('',(0.963525491562421,1.55,0.267616567329818));
#14574=CARTESIAN_POINT('',(0.125,1.55,-0.21650635094611));
#14575=CARTESIAN_POINT('Ctrl Pts',(0.963525491562421,1.55,0.267616567329818));
#14576=CARTESIAN_POINT('Ctrl Pts',(0.963525491562421,1.5815373526696,0.267616567329818));
#14577=CARTESIAN_POINT('Ctrl Pts',(0.961833761492987,1.61508042700263,0.273949373987484));
#14578=CARTESIAN_POINT('Ctrl Pts',(0.954308486908894,1.67663267125761,0.299111603474268));
#14579=CARTESIAN_POINT('Ctrl Pts',(0.948394987258249,1.70465411363682,0.31788699900678));
#14580=CARTESIAN_POINT('Ctrl Pts',(0.933155485613026,1.74889618382539,0.360174810895352));
#14581=CARTESIAN_POINT('Ctrl Pts',(0.92278792026947,1.76811531482682,0.386546956384144));
#14582=CARTESIAN_POINT('Ctrl Pts',(0.897143218189782,1.79367084275751,0.442820664919227));
#14583=CARTESIAN_POINT('Ctrl Pts',(0.881791875377343,1.8,0.472691670144998));
#14584=CARTESIAN_POINT('Ctrl Pts',(0.850258932191534,1.8,0.527308329855003));
#14585=CARTESIAN_POINT('Ctrl Pts',(0.832065554235658,1.79367084275751,0.555538485325664));
#14586=CARTESIAN_POINT('Ctrl Pts',(0.796153444118959,1.76811531482682,0.605884303066698));
#14587=CARTESIAN_POINT('Ctrl Pts',(0.778498278845144,1.74889618382539,0.62804895077401));
#14588=CARTESIAN_POINT('Ctrl Pts',(0.749495710301794,1.70465411363682,0.662390652284073));
#14589=CARTESIAN_POINT('Ctrl Pts',(0.73619249062986,1.67663267125761,0.676899590973058));
#14590=CARTESIAN_POINT('Ctrl Pts',(0.718163997970498,1.61508042700263,0.695997784676728));
#14591=CARTESIAN_POINT('Ctrl Pts',(0.713525491562421,1.5815373526696,0.700629269222037));
#14592=CARTESIAN_POINT('Ctrl Pts',(0.713525491562421,1.5184626473304,0.700629269222037));
#14593=CARTESIAN_POINT('Ctrl Pts',(0.718163997970498,1.48491957299737,0.695997784676728));
#14594=CARTESIAN_POINT('Ctrl Pts',(0.73619249062986,1.42336732874239,0.676899590973058));
#14595=CARTESIAN_POINT('Ctrl Pts',(0.749495710301794,1.39534588636318,0.662390652284073));
#14596=CARTESIAN_POINT('Ctrl Pts',(0.778498278845144,1.35110381617461,0.62804895077401));
#14597=CARTESIAN_POINT('Ctrl Pts',(0.796153444118959,1.33188468517318,0.605884303066698));
#14598=CARTESIAN_POINT('Ctrl Pts',(0.832065554235658,1.30632915724249,0.555538485325664));
#14599=CARTESIAN_POINT('Ctrl Pts',(0.850258932191534,1.3,0.527308329855003));
#14600=CARTESIAN_POINT('Ctrl Pts',(0.881791875377343,1.3,0.472691670144998));
#14601=CARTESIAN_POINT('Ctrl Pts',(0.897143218189782,1.30632915724249,0.442820664919227));
#14602=CARTESIAN_POINT('Ctrl Pts',(0.92278792026947,1.33188468517318,0.386546956384144));
#14603=CARTESIAN_POINT('Ctrl Pts',(0.933155485613026,1.35110381617461,0.360174810895352));
#14604=CARTESIAN_POINT('Ctrl Pts',(0.948394987258249,1.39534588636318,0.31788699900678));
#14605=CARTESIAN_POINT('Ctrl Pts',(0.954308486908894,1.42336732874239,0.299111603474268));
#14606=CARTESIAN_POINT('Ctrl Pts',(0.961833761492987,1.48491957299738,0.273949373987484));
#14607=CARTESIAN_POINT('Ctrl Pts',(0.963525491562421,1.5184626473304,0.267616567329818));
#14608=CARTESIAN_POINT('Ctrl Pts',(0.963525491562421,1.55,0.267616567329818));
#14609=CARTESIAN_POINT('Origin',(0.,1.55,0.));
#14610=CARTESIAN_POINT('',(-0.713525491562421,1.55,-0.700629269222037));
#14611=CARTESIAN_POINT('Ctrl Pts',(-0.713525491562421,1.55,-0.700629269222037));
#14612=CARTESIAN_POINT('Ctrl Pts',(-0.713525491562421,1.5184626473304,-0.700629269222037));
#14613=CARTESIAN_POINT('Ctrl Pts',(-0.718163997970498,1.48491957299737,
-0.695997784676728));
#14614=CARTESIAN_POINT('Ctrl Pts',(-0.73619249062986,1.42336732874239,-0.676899590973058));
#14615=CARTESIAN_POINT('Ctrl Pts',(-0.749495710301794,1.39534588636318,
-0.662390652284073));
#14616=CARTESIAN_POINT('Ctrl Pts',(-0.778498278845144,1.35110381617461,
-0.62804895077401));
#14617=CARTESIAN_POINT('Ctrl Pts',(-0.796153444118959,1.33188468517318,
-0.605884303066698));
#14618=CARTESIAN_POINT('Ctrl Pts',(-0.832065554235658,1.30632915724249,
-0.555538485325664));
#14619=CARTESIAN_POINT('Ctrl Pts',(-0.850258932191534,1.3,-0.527308329855003));
#14620=CARTESIAN_POINT('Ctrl Pts',(-0.881791875377343,1.3,-0.472691670144998));
#14621=CARTESIAN_POINT('Ctrl Pts',(-0.897143218189782,1.30632915724249,
-0.442820664919227));
#14622=CARTESIAN_POINT('Ctrl Pts',(-0.92278792026947,1.33188468517318,-0.386546956384144));
#14623=CARTESIAN_POINT('Ctrl Pts',(-0.933155485613026,1.35110381617461,
-0.360174810895352));
#14624=CARTESIAN_POINT('Ctrl Pts',(-0.948394987258249,1.39534588636318,
-0.31788699900678));
#14625=CARTESIAN_POINT('Ctrl Pts',(-0.954308486908894,1.42336732874239,
-0.299111603474268));
#14626=CARTESIAN_POINT('Ctrl Pts',(-0.961833761492986,1.48491957299737,
-0.273949373987484));
#14627=CARTESIAN_POINT('Ctrl Pts',(-0.963525491562421,1.5184626473304,-0.267616567329818));
#14628=CARTESIAN_POINT('Ctrl Pts',(-0.963525491562421,1.5815373526696,-0.267616567329818));
#14629=CARTESIAN_POINT('Ctrl Pts',(-0.961833761492986,1.61508042700263,
-0.273949373987484));
#14630=CARTESIAN_POINT('Ctrl Pts',(-0.954308486908894,1.67663267125761,
-0.299111603474268));
#14631=CARTESIAN_POINT('Ctrl Pts',(-0.948394987258249,1.70465411363682,
-0.31788699900678));
#14632=CARTESIAN_POINT('Ctrl Pts',(-0.933155485613026,1.74889618382539,
-0.360174810895352));
#14633=CARTESIAN_POINT('Ctrl Pts',(-0.92278792026947,1.76811531482682,-0.386546956384144));
#14634=CARTESIAN_POINT('Ctrl Pts',(-0.897143218189782,1.79367084275751,
-0.442820664919227));
#14635=CARTESIAN_POINT('Ctrl Pts',(-0.881791875377343,1.8,-0.472691670144998));
#14636=CARTESIAN_POINT('Ctrl Pts',(-0.850258932191534,1.8,-0.527308329855003));
#14637=CARTESIAN_POINT('Ctrl Pts',(-0.832065554235658,1.79367084275751,
-0.555538485325664));
#14638=CARTESIAN_POINT('Ctrl Pts',(-0.796153444118959,1.76811531482682,
-0.605884303066698));
#14639=CARTESIAN_POINT('Ctrl Pts',(-0.778498278845144,1.74889618382539,
-0.62804895077401));
#14640=CARTESIAN_POINT('Ctrl Pts',(-0.749495710301794,1.70465411363682,
-0.662390652284073));
#14641=CARTESIAN_POINT('Ctrl Pts',(-0.73619249062986,1.67663267125761,-0.676899590973058));
#14642=CARTESIAN_POINT('Ctrl Pts',(-0.718163997970498,1.61508042700263,
-0.695997784676728));
#14643=CARTESIAN_POINT('Ctrl Pts',(-0.713525491562421,1.5815373526696,-0.700629269222037));
#14644=CARTESIAN_POINT('Ctrl Pts',(-0.713525491562421,1.55,-0.700629269222037));
#14645=CARTESIAN_POINT('',(-1.28744468918255,1.55,-1.03198167246111));
#14646=CARTESIAN_POINT('',(0.125,1.55,-0.21650635094611));
#14647=CARTESIAN_POINT('',(-1.42894191624432,1.3,-0.825000000000001));
#14648=CARTESIAN_POINT('Ctrl Pts',(-1.42894191624432,1.3,-0.825000000000001));
#14649=CARTESIAN_POINT('Ctrl Pts',(-1.4132207435299,1.3,-0.852229869895949));
#14650=CARTESIAN_POINT('Ctrl Pts',(-1.39561049050871,1.30629366210296,-0.880751161609749));
#14651=CARTESIAN_POINT('Ctrl Pts',(-1.36172049302549,1.33182222741682,-0.932292094146256));
#14652=CARTESIAN_POINT('Ctrl Pts',(-1.34548213209931,1.35105447038507,-0.955340251466735));
#14653=CARTESIAN_POINT('Ctrl Pts',(-1.31917543061769,1.39539254159618,-0.991349264982991));
#14654=CARTESIAN_POINT('Ctrl Pts',(-1.30734972067592,1.42347183818157,-1.00672880483252));
#14655=CARTESIAN_POINT('Ctrl Pts',(-1.29146042158868,1.48505200040818,-1.02703269653942));
#14656=CARTESIAN_POINT('Ctrl Pts',(-1.28744468918255,1.51855708359447,-1.03198167246111));
#14657=CARTESIAN_POINT('Ctrl Pts',(-1.28744468918255,1.55,-1.03198167246111));
#14658=CARTESIAN_POINT('',(-1.42894191624432,1.8,-0.825000000000001));
#14659=CARTESIAN_POINT('Ctrl Pts',(-1.42894191624432,1.8,-0.825000000000001));
#14660=CARTESIAN_POINT('Ctrl Pts',(-1.44466308895875,1.8,-0.797770130104052));
#14661=CARTESIAN_POINT('Ctrl Pts',(-1.46055812562105,1.79370633789704,-0.768258557763732));
#14662=CARTESIAN_POINT('Ctrl Pts',(-1.48824888379079,1.76817777258318,-0.713138492740816));
#14663=CARTESIAN_POINT('Ctrl Pts',(-1.50008999307766,1.74894552961493,-0.687551581002689));
#14664=CARTESIAN_POINT('Ctrl Pts',(-1.51812136280714,1.70460745840382,-0.646764802471699));
#14665=CARTESIAN_POINT('Ctrl Pts',(-1.52552758004446,1.67652816181843,-0.628833667319578));
#14666=CARTESIAN_POINT('Ctrl Pts',(-1.53516661651472,1.61494799959182,-0.60492118480825));
#14667=CARTESIAN_POINT('Ctrl Pts',(-1.53744468918255,1.58144291640553,-0.598968970568896));
#14668=CARTESIAN_POINT('Ctrl Pts',(-1.53744468918255,1.51855708359447,-0.598968970568896));
#14669=CARTESIAN_POINT('Ctrl Pts',(-1.53516661651472,1.48505200040818,-0.60492118480825));
#14670=CARTESIAN_POINT('Ctrl Pts',(-1.52552758004446,1.42347183818157,-0.628833667319578));
#14671=CARTESIAN_POINT('Ctrl Pts',(-1.51812136280714,1.39539254159618,-0.646764802471699));
#14672=CARTESIAN_POINT('Ctrl Pts',(-1.50008999307766,1.35105447038507,-0.687551581002689));
#14673=CARTESIAN_POINT('Ctrl Pts',(-1.48824888379079,1.33182222741682,-0.713138492740816));
#14674=CARTESIAN_POINT('Ctrl Pts',(-1.46055812562105,1.30629366210296,-0.768258557763732));
#14675=CARTESIAN_POINT('Ctrl Pts',(-1.44466308895875,1.3,-0.797770130104052));
#14676=CARTESIAN_POINT('Ctrl Pts',(-1.42894191624432,1.3,-0.825000000000001));
#14677=CARTESIAN_POINT('Ctrl Pts',(-1.28744468918255,1.55,-1.03198167246111));
#14678=CARTESIAN_POINT('Ctrl Pts',(-1.28744468918255,1.58144291640553,-1.03198167246111));
#14679=CARTESIAN_POINT('Ctrl Pts',(-1.29146042158868,1.61494799959182,-1.02703269653942));
#14680=CARTESIAN_POINT('Ctrl Pts',(-1.30734972067592,1.67652816181843,-1.00672880483252));
#14681=CARTESIAN_POINT('Ctrl Pts',(-1.31917543061769,1.70460745840382,-0.991349264982991));
#14682=CARTESIAN_POINT('Ctrl Pts',(-1.34548213209931,1.74894552961493,-0.955340251466734));
#14683=CARTESIAN_POINT('Ctrl Pts',(-1.36172049302549,1.76817777258318,-0.932292094146256));
#14684=CARTESIAN_POINT('Ctrl Pts',(-1.39561049050871,1.79370633789704,-0.880751161609749));
#14685=CARTESIAN_POINT('Ctrl Pts',(-1.4132207435299,1.8,-0.852229869895949));
#14686=CARTESIAN_POINT('Ctrl Pts',(-1.42894191624432,1.8,-0.825000000000001));
#14687=CARTESIAN_POINT('Origin',(0.,1.55,0.));
#14688=CARTESIAN_POINT('',(-1.65,0.85,-2.02066721859313E-16));
#14689=CARTESIAN_POINT('Origin',(0.,0.85,0.));
#14690=CARTESIAN_POINT('',(-1.65,2.25,-2.02066721859313E-16));
#14691=CARTESIAN_POINT('',(-1.65,1.55,-2.02066721859313E-16));
#14692=CARTESIAN_POINT('Origin',(0.,2.25,0.));
#14693=CARTESIAN_POINT('',(-1.42894191624432,1.3,0.825));
#14694=CARTESIAN_POINT('',(-1.42894191624432,1.8,0.825));
#14695=CARTESIAN_POINT('Ctrl Pts',(-1.42894191624432,1.3,0.825));
#14696=CARTESIAN_POINT('Ctrl Pts',(-1.44466308895875,1.3,0.797770130104051));
#14697=CARTESIAN_POINT('Ctrl Pts',(-1.46055812562105,1.30629366210296,0.768258557763731));
#14698=CARTESIAN_POINT('Ctrl Pts',(-1.48824888379079,1.33182222741682,0.713138492740815));
#14699=CARTESIAN_POINT('Ctrl Pts',(-1.50008999307766,1.35105447038507,0.687551581002688));
#14700=CARTESIAN_POINT('Ctrl Pts',(-1.51812136280714,1.39539254159618,0.646764802471698));
#14701=CARTESIAN_POINT('Ctrl Pts',(-1.52552758004446,1.42347183818157,0.628833667319577));
#14702=CARTESIAN_POINT('Ctrl Pts',(-1.53516661651472,1.48505200040818,0.604921184808249));
#14703=CARTESIAN_POINT('Ctrl Pts',(-1.53744468918255,1.51855708359447,0.598968970568895));
#14704=CARTESIAN_POINT('Ctrl Pts',(-1.53744468918255,1.58144291640553,0.598968970568895));
#14705=CARTESIAN_POINT('Ctrl Pts',(-1.53516661651472,1.61494799959182,0.604921184808249));
#14706=CARTESIAN_POINT('Ctrl Pts',(-1.52552758004446,1.67652816181843,0.628833667319577));
#14707=CARTESIAN_POINT('Ctrl Pts',(-1.51812136280714,1.70460745840382,0.646764802471698));
#14708=CARTESIAN_POINT('Ctrl Pts',(-1.50008999307766,1.74894552961493,0.687551581002688));
#14709=CARTESIAN_POINT('Ctrl Pts',(-1.48824888379079,1.76817777258318,0.713138492740815));
#14710=CARTESIAN_POINT('Ctrl Pts',(-1.46055812562105,1.79370633789704,0.768258557763731));
#14711=CARTESIAN_POINT('Ctrl Pts',(-1.44466308895875,1.8,0.797770130104051));
#14712=CARTESIAN_POINT('Ctrl Pts',(-1.42894191624432,1.8,0.825));
#14713=CARTESIAN_POINT('',(-1.28744468918255,1.55,1.03198167246111));
#14714=CARTESIAN_POINT('Ctrl Pts',(-1.42894191624432,1.8,0.825));
#14715=CARTESIAN_POINT('Ctrl Pts',(-1.4132207435299,1.8,0.852229869895948));
#14716=CARTESIAN_POINT('Ctrl Pts',(-1.39561049050871,1.79370633789704,0.880751161609747));
#14717=CARTESIAN_POINT('Ctrl Pts',(-1.36172049302549,1.76817777258318,0.932292094146255));
#14718=CARTESIAN_POINT('Ctrl Pts',(-1.34548213209931,1.74894552961493,0.955340251466733));
#14719=CARTESIAN_POINT('Ctrl Pts',(-1.31917543061769,1.70460745840382,0.991349264982989));
#14720=CARTESIAN_POINT('Ctrl Pts',(-1.30734972067592,1.67652816181843,1.00672880483252));
#14721=CARTESIAN_POINT('Ctrl Pts',(-1.29146042158868,1.61494799959182,1.02703269653942));
#14722=CARTESIAN_POINT('Ctrl Pts',(-1.28744468918255,1.58144291640553,1.03198167246111));
#14723=CARTESIAN_POINT('Ctrl Pts',(-1.28744468918255,1.55,1.03198167246111));
#14724=CARTESIAN_POINT('Ctrl Pts',(-1.28744468918255,1.55,1.03198167246111));
#14725=CARTESIAN_POINT('Ctrl Pts',(-1.28744468918255,1.51855708359447,1.03198167246111));
#14726=CARTESIAN_POINT('Ctrl Pts',(-1.29146042158868,1.48505200040818,1.02703269653942));
#14727=CARTESIAN_POINT('Ctrl Pts',(-1.30734972067592,1.42347183818157,1.00672880483252));
#14728=CARTESIAN_POINT('Ctrl Pts',(-1.31917543061769,1.39539254159618,0.99134926498299));
#14729=CARTESIAN_POINT('Ctrl Pts',(-1.34548213209931,1.35105447038508,0.955340251466733));
#14730=CARTESIAN_POINT('Ctrl Pts',(-1.36172049302549,1.33182222741682,0.932292094146255));
#14731=CARTESIAN_POINT('Ctrl Pts',(-1.39561049050871,1.30629366210296,0.880751161609748));
#14732=CARTESIAN_POINT('Ctrl Pts',(-1.4132207435299,1.3,0.852229869895949));
#14733=CARTESIAN_POINT('Ctrl Pts',(-1.42894191624432,1.3,0.825));
#14734=CARTESIAN_POINT('',(1.42894191624432,1.8,-0.825));
#14735=CARTESIAN_POINT('',(1.42894191624432,1.3,-0.825));
#14736=CARTESIAN_POINT('Ctrl Pts',(1.42894191624432,1.8,-0.825));
#14737=CARTESIAN_POINT('Ctrl Pts',(1.4132207435299,1.8,-0.852229869895949));
#14738=CARTESIAN_POINT('Ctrl Pts',(1.39561049050871,1.79370633789704,-0.880751161609748));
#14739=CARTESIAN_POINT('Ctrl Pts',(1.36172049302549,1.76817777258318,-0.932292094146255));
#14740=CARTESIAN_POINT('Ctrl Pts',(1.34548213209931,1.74894552961493,-0.955340251466734));
#14741=CARTESIAN_POINT('Ctrl Pts',(1.31917543061769,1.70460745840382,-0.99134926498299));
#14742=CARTESIAN_POINT('Ctrl Pts',(1.30734972067592,1.67652816181843,-1.00672880483252));
#14743=CARTESIAN_POINT('Ctrl Pts',(1.29146042158868,1.61494799959182,-1.02703269653942));
#14744=CARTESIAN_POINT('Ctrl Pts',(1.28744468918255,1.58144291640553,-1.03198167246111));
#14745=CARTESIAN_POINT('Ctrl Pts',(1.28744468918255,1.51855708359447,-1.03198167246111));
#14746=CARTESIAN_POINT('Ctrl Pts',(1.29146042158868,1.48505200040818,-1.02703269653942));
#14747=CARTESIAN_POINT('Ctrl Pts',(1.30734972067592,1.42347183818157,-1.00672880483252));
#14748=CARTESIAN_POINT('Ctrl Pts',(1.31917543061769,1.39539254159618,-0.99134926498299));
#14749=CARTESIAN_POINT('Ctrl Pts',(1.34548213209931,1.35105447038507,-0.955340251466734));
#14750=CARTESIAN_POINT('Ctrl Pts',(1.36172049302549,1.33182222741682,-0.932292094146255));
#14751=CARTESIAN_POINT('Ctrl Pts',(1.39561049050871,1.30629366210296,-0.880751161609748));
#14752=CARTESIAN_POINT('Ctrl Pts',(1.4132207435299,1.3,-0.852229869895948));
#14753=CARTESIAN_POINT('Ctrl Pts',(1.42894191624432,1.3,-0.825));
#14754=CARTESIAN_POINT('',(1.53744468918255,1.55,-0.598968970568895));
#14755=CARTESIAN_POINT('Ctrl Pts',(1.42894191624432,1.3,-0.825));
#14756=CARTESIAN_POINT('Ctrl Pts',(1.44466308895875,1.3,-0.797770130104051));
#14757=CARTESIAN_POINT('Ctrl Pts',(1.46055812562105,1.30629366210296,-0.768258557763731));
#14758=CARTESIAN_POINT('Ctrl Pts',(1.48824888379079,1.33182222741682,-0.713138492740815));
#14759=CARTESIAN_POINT('Ctrl Pts',(1.50008999307766,1.35105447038507,-0.687551581002688));
#14760=CARTESIAN_POINT('Ctrl Pts',(1.51812136280714,1.39539254159618,-0.646764802471698));
#14761=CARTESIAN_POINT('Ctrl Pts',(1.52552758004446,1.42347183818157,-0.628833667319577));
#14762=CARTESIAN_POINT('Ctrl Pts',(1.53516661651472,1.48505200040818,-0.604921184808249));
#14763=CARTESIAN_POINT('Ctrl Pts',(1.53744468918255,1.51855708359447,-0.598968970568895));
#14764=CARTESIAN_POINT('Ctrl Pts',(1.53744468918255,1.55,-0.598968970568895));
#14765=CARTESIAN_POINT('Ctrl Pts',(1.53744468918255,1.55,-0.598968970568895));
#14766=CARTESIAN_POINT('Ctrl Pts',(1.53744468918255,1.58144291640553,-0.598968970568895));
#14767=CARTESIAN_POINT('Ctrl Pts',(1.53516661651472,1.61494799959182,-0.604921184808249));
#14768=CARTESIAN_POINT('Ctrl Pts',(1.52552758004446,1.67652816181843,-0.628833667319577));
#14769=CARTESIAN_POINT('Ctrl Pts',(1.51812136280714,1.70460745840382,-0.646764802471698));
#14770=CARTESIAN_POINT('Ctrl Pts',(1.50008999307766,1.74894552961493,-0.687551581002688));
#14771=CARTESIAN_POINT('Ctrl Pts',(1.48824888379079,1.76817777258318,-0.713138492740815));
#14772=CARTESIAN_POINT('Ctrl Pts',(1.46055812562105,1.79370633789704,-0.768258557763731));
#14773=CARTESIAN_POINT('Ctrl Pts',(1.44466308895875,1.8,-0.797770130104051));
#14774=CARTESIAN_POINT('Ctrl Pts',(1.42894191624432,1.8,-0.825));
#14775=CARTESIAN_POINT('',(0.,1.3,-1.65));
#14776=CARTESIAN_POINT('',(0.,1.8,-1.65));
#14777=CARTESIAN_POINT('Ctrl Pts',(1.38777878078145E-17,1.3,-1.65));
#14778=CARTESIAN_POINT('Ctrl Pts',(0.0314423454288489,1.3,-1.65));
#14779=CARTESIAN_POINT('Ctrl Pts',(0.0649476351123396,1.30629366210296,
-1.64900971937348));
#14780=CARTESIAN_POINT('Ctrl Pts',(0.126528390765307,1.33182222741682,-1.64543058688707));
#14781=CARTESIAN_POINT('Ctrl Pts',(0.154607860978348,1.35105447038507,-1.64289183246942));
#14782=CARTESIAN_POINT('Ctrl Pts',(0.198945932189457,1.39539254159618,-1.63811406745469));
#14783=CARTESIAN_POINT('Ctrl Pts',(0.218177859368546,1.42347183818157,-1.63556247215209));
#14784=CARTESIAN_POINT('Ctrl Pts',(0.243706194926033,1.48505200040818,-1.63195388134767));
#14785=CARTESIAN_POINT('Ctrl Pts',(0.25,1.51855708359447,-1.63095064303001));
#14786=CARTESIAN_POINT('Ctrl Pts',(0.25,1.58144291640553,-1.63095064303001));
#14787=CARTESIAN_POINT('Ctrl Pts',(0.243706194926033,1.61494799959182,-1.63195388134767));
#14788=CARTESIAN_POINT('Ctrl Pts',(0.218177859368546,1.67652816181843,-1.63556247215209));
#14789=CARTESIAN_POINT('Ctrl Pts',(0.198945932189457,1.70460745840382,-1.63811406745469));
#14790=CARTESIAN_POINT('Ctrl Pts',(0.154607860978349,1.74894552961493,-1.64289183246942));
#14791=CARTESIAN_POINT('Ctrl Pts',(0.126528390765307,1.76817777258318,-1.64543058688707));
#14792=CARTESIAN_POINT('Ctrl Pts',(0.0649476351123398,1.79370633789704,
-1.64900971937348));
#14793=CARTESIAN_POINT('Ctrl Pts',(0.031442345428849,1.8,-1.65));
#14794=CARTESIAN_POINT('Ctrl Pts',(7.63278329429795E-17,1.8,-1.65));
#14795=CARTESIAN_POINT('',(-0.25,1.55,-1.63095064303001));
#14796=CARTESIAN_POINT('Ctrl Pts',(9.0205620750794E-17,1.8,-1.65));
#14797=CARTESIAN_POINT('Ctrl Pts',(-0.0314423454288488,1.8,-1.65));
#14798=CARTESIAN_POINT('Ctrl Pts',(-0.0649476351123396,1.79370633789704,
-1.64900971937348));
#14799=CARTESIAN_POINT('Ctrl Pts',(-0.126528390765307,1.76817777258318,
-1.64543058688707));
#14800=CARTESIAN_POINT('Ctrl Pts',(-0.154607860978348,1.74894552961493,
-1.64289183246942));
#14801=CARTESIAN_POINT('Ctrl Pts',(-0.198945932189456,1.70460745840382,
-1.63811406745469));
#14802=CARTESIAN_POINT('Ctrl Pts',(-0.218177859368546,1.67652816181843,
-1.63556247215209));
#14803=CARTESIAN_POINT('Ctrl Pts',(-0.243706194926033,1.61494799959182,
-1.63195388134767));
#14804=CARTESIAN_POINT('Ctrl Pts',(-0.25,1.58144291640553,-1.63095064303001));
#14805=CARTESIAN_POINT('Ctrl Pts',(-0.25,1.55,-1.63095064303001));
#14806=CARTESIAN_POINT('Ctrl Pts',(-0.25,1.55,-1.63095064303001));
#14807=CARTESIAN_POINT('Ctrl Pts',(-0.25,1.51855708359447,-1.63095064303001));
#14808=CARTESIAN_POINT('Ctrl Pts',(-0.243706194926033,1.48505200040818,
-1.63195388134767));
#14809=CARTESIAN_POINT('Ctrl Pts',(-0.218177859368546,1.42347183818157,
-1.63556247215209));
#14810=CARTESIAN_POINT('Ctrl Pts',(-0.198945932189457,1.39539254159618,
-1.63811406745469));
#14811=CARTESIAN_POINT('Ctrl Pts',(-0.154607860978349,1.35105447038507,
-1.64289183246942));
#14812=CARTESIAN_POINT('Ctrl Pts',(-0.126528390765307,1.33182222741682,
-1.64543058688707));
#14813=CARTESIAN_POINT('Ctrl Pts',(-0.0649476351123398,1.30629366210296,
-1.64900971937348));
#14814=CARTESIAN_POINT('Ctrl Pts',(-0.031442345428849,1.3,-1.65));
#14815=CARTESIAN_POINT('Ctrl Pts',(-4.85722573273506E-17,1.3,-1.65));
#14816=CARTESIAN_POINT('',(0.,1.8,1.65));
#14817=CARTESIAN_POINT('',(0.,1.3,1.65));
#14818=CARTESIAN_POINT('Ctrl Pts',(8.32667268468867E-17,1.8,1.65));
#14819=CARTESIAN_POINT('Ctrl Pts',(0.031442345428849,1.8,1.65));
#14820=CARTESIAN_POINT('Ctrl Pts',(0.0649476351123398,1.79370633789704,
1.64900971937348));
#14821=CARTESIAN_POINT('Ctrl Pts',(0.126528390765307,1.76817777258318,1.64543058688707));
#14822=CARTESIAN_POINT('Ctrl Pts',(0.154607860978349,1.74894552961493,1.64289183246942));
#14823=CARTESIAN_POINT('Ctrl Pts',(0.198945932189457,1.70460745840382,1.63811406745469));
#14824=CARTESIAN_POINT('Ctrl Pts',(0.218177859368546,1.67652816181843,1.63556247215209));
#14825=CARTESIAN_POINT('Ctrl Pts',(0.243706194926033,1.61494799959182,1.63195388134767));
#14826=CARTESIAN_POINT('Ctrl Pts',(0.25,1.58144291640553,1.63095064303001));
#14827=CARTESIAN_POINT('Ctrl Pts',(0.25,1.51855708359447,1.63095064303001));
#14828=CARTESIAN_POINT('Ctrl Pts',(0.243706194926033,1.48505200040818,1.63195388134767));
#14829=CARTESIAN_POINT('Ctrl Pts',(0.218177859368546,1.42347183818157,1.63556247215209));
#14830=CARTESIAN_POINT('Ctrl Pts',(0.198945932189457,1.39539254159618,1.63811406745469));
#14831=CARTESIAN_POINT('Ctrl Pts',(0.154607860978348,1.35105447038507,1.64289183246942));
#14832=CARTESIAN_POINT('Ctrl Pts',(0.126528390765307,1.33182222741682,1.64543058688707));
#14833=CARTESIAN_POINT('Ctrl Pts',(0.0649476351123397,1.30629366210296,
1.64900971937348));
#14834=CARTESIAN_POINT('Ctrl Pts',(0.0314423454288488,1.3,1.65));
#14835=CARTESIAN_POINT('Ctrl Pts',(-1.38777878078145E-17,1.3,1.65));
#14836=CARTESIAN_POINT('',(-0.25,1.55,1.63095064303001));
#14837=CARTESIAN_POINT('Ctrl Pts',(-5.55111512312578E-17,1.3,1.65));
#14838=CARTESIAN_POINT('Ctrl Pts',(-0.031442345428849,1.3,1.65));
#14839=CARTESIAN_POINT('Ctrl Pts',(-0.0649476351123398,1.30629366210296,
1.64900971937348));
#14840=CARTESIAN_POINT('Ctrl Pts',(-0.126528390765307,1.33182222741682,
1.64543058688707));
#14841=CARTESIAN_POINT('Ctrl Pts',(-0.154607860978349,1.35105447038507,
1.64289183246942));
#14842=CARTESIAN_POINT('Ctrl Pts',(-0.198945932189457,1.39539254159618,
1.63811406745469));
#14843=CARTESIAN_POINT('Ctrl Pts',(-0.218177859368546,1.42347183818157,
1.63556247215209));
#14844=CARTESIAN_POINT('Ctrl Pts',(-0.243706194926033,1.48505200040818,
1.63195388134767));
#14845=CARTESIAN_POINT('Ctrl Pts',(-0.25,1.51855708359447,1.63095064303001));
#14846=CARTESIAN_POINT('Ctrl Pts',(-0.25,1.55,1.63095064303001));
#14847=CARTESIAN_POINT('Ctrl Pts',(-0.25,1.55,1.63095064303001));
#14848=CARTESIAN_POINT('Ctrl Pts',(-0.25,1.58144291640553,1.63095064303001));
#14849=CARTESIAN_POINT('Ctrl Pts',(-0.243706194926033,1.61494799959182,
1.63195388134767));
#14850=CARTESIAN_POINT('Ctrl Pts',(-0.218177859368546,1.67652816181843,
1.63556247215209));
#14851=CARTESIAN_POINT('Ctrl Pts',(-0.198945932189456,1.70460745840382,
1.63811406745469));
#14852=CARTESIAN_POINT('Ctrl Pts',(-0.154607860978348,1.74894552961493,
1.64289183246942));
#14853=CARTESIAN_POINT('Ctrl Pts',(-0.126528390765307,1.76817777258318,
1.64543058688707));
#14854=CARTESIAN_POINT('Ctrl Pts',(-0.0649476351123396,1.79370633789704,
1.64900971937348));
#14855=CARTESIAN_POINT('Ctrl Pts',(-0.0314423454288488,1.8,1.65));
#14856=CARTESIAN_POINT('Ctrl Pts',(7.63278329429795E-17,1.8,1.65));
#14857=CARTESIAN_POINT('Origin',(0.,1.55,0.));
#14858=CARTESIAN_POINT('',(-0.713525491562421,1.55,0.700629269222037));
#14859=CARTESIAN_POINT('',(0.125,1.55,0.21650635094611));
#14860=CARTESIAN_POINT('Ctrl Pts',(-0.713525491562421,1.55,0.700629269222037));
#14861=CARTESIAN_POINT('Ctrl Pts',(-0.713525491562421,1.5815373526696,0.700629269222037));
#14862=CARTESIAN_POINT('Ctrl Pts',(-0.718163997970498,1.61508042700263,
0.695997784676727));
#14863=CARTESIAN_POINT('Ctrl Pts',(-0.73619249062986,1.67663267125761,0.676899590973058));
#14864=CARTESIAN_POINT('Ctrl Pts',(-0.749495710301795,1.70465411363682,
0.662390652284073));
#14865=CARTESIAN_POINT('Ctrl Pts',(-0.778498278845144,1.74889618382539,
0.628048950774009));
#14866=CARTESIAN_POINT('Ctrl Pts',(-0.796153444118959,1.76811531482682,
0.605884303066698));
#14867=CARTESIAN_POINT('Ctrl Pts',(-0.832065554235658,1.79367084275751,
0.555538485325663));
#14868=CARTESIAN_POINT('Ctrl Pts',(-0.850258932191534,1.8,0.527308329855002));
#14869=CARTESIAN_POINT('Ctrl Pts',(-0.881791875377343,1.8,0.472691670144998));
#14870=CARTESIAN_POINT('Ctrl Pts',(-0.897143218189782,1.79367084275751,
0.442820664919227));
#14871=CARTESIAN_POINT('Ctrl Pts',(-0.92278792026947,1.76811531482682,0.386546956384144));
#14872=CARTESIAN_POINT('Ctrl Pts',(-0.933155485613026,1.74889618382539,
0.360174810895352));
#14873=CARTESIAN_POINT('Ctrl Pts',(-0.948394987258249,1.70465411363682,
0.31788699900678));
#14874=CARTESIAN_POINT('Ctrl Pts',(-0.954308486908894,1.67663267125761,
0.299111603474267));
#14875=CARTESIAN_POINT('Ctrl Pts',(-0.961833761492987,1.61508042700263,
0.273949373987484));
#14876=CARTESIAN_POINT('Ctrl Pts',(-0.963525491562421,1.5815373526696,0.267616567329817));
#14877=CARTESIAN_POINT('Ctrl Pts',(-0.963525491562421,1.5184626473304,0.267616567329817));
#14878=CARTESIAN_POINT('Ctrl Pts',(-0.961833761492987,1.48491957299737,
0.273949373987484));
#14879=CARTESIAN_POINT('Ctrl Pts',(-0.954308486908894,1.42336732874239,
0.299111603474267));
#14880=CARTESIAN_POINT('Ctrl Pts',(-0.948394987258249,1.39534588636318,
0.31788699900678));
#14881=CARTESIAN_POINT('Ctrl Pts',(-0.933155485613026,1.35110381617461,
0.360174810895352));
#14882=CARTESIAN_POINT('Ctrl Pts',(-0.92278792026947,1.33188468517318,0.386546956384144));
#14883=CARTESIAN_POINT('Ctrl Pts',(-0.897143218189782,1.30632915724249,
0.442820664919227));
#14884=CARTESIAN_POINT('Ctrl Pts',(-0.881791875377343,1.3,0.472691670144998));
#14885=CARTESIAN_POINT('Ctrl Pts',(-0.850258932191534,1.3,0.527308329855002));
#14886=CARTESIAN_POINT('Ctrl Pts',(-0.832065554235658,1.30632915724249,
0.555538485325663));
#14887=CARTESIAN_POINT('Ctrl Pts',(-0.796153444118959,1.33188468517318,
0.605884303066698));
#14888=CARTESIAN_POINT('Ctrl Pts',(-0.778498278845144,1.35110381617461,
0.628048950774009));
#14889=CARTESIAN_POINT('Ctrl Pts',(-0.749495710301795,1.39534588636318,
0.662390652284073));
#14890=CARTESIAN_POINT('Ctrl Pts',(-0.73619249062986,1.42336732874239,0.676899590973058));
#14891=CARTESIAN_POINT('Ctrl Pts',(-0.718163997970498,1.48491957299737,
0.695997784676727));
#14892=CARTESIAN_POINT('Ctrl Pts',(-0.713525491562421,1.5184626473304,0.700629269222037));
#14893=CARTESIAN_POINT('Ctrl Pts',(-0.713525491562421,1.55,0.700629269222037));
#14894=CARTESIAN_POINT('Origin',(0.,1.55,0.));
#14895=CARTESIAN_POINT('',(0.963525491562421,1.55,-0.267616567329817));
#14896=CARTESIAN_POINT('Ctrl Pts',(0.963525491562421,1.55,-0.267616567329817));
#14897=CARTESIAN_POINT('Ctrl Pts',(0.963525491562421,1.5184626473304,-0.267616567329817));
#14898=CARTESIAN_POINT('Ctrl Pts',(0.961833761492987,1.48491957299737,-0.273949373987484));
#14899=CARTESIAN_POINT('Ctrl Pts',(0.954308486908894,1.42336732874239,-0.299111603474267));
#14900=CARTESIAN_POINT('Ctrl Pts',(0.948394987258249,1.39534588636318,-0.31788699900678));
#14901=CARTESIAN_POINT('Ctrl Pts',(0.933155485613026,1.35110381617461,-0.360174810895352));
#14902=CARTESIAN_POINT('Ctrl Pts',(0.92278792026947,1.33188468517318,-0.386546956384144));
#14903=CARTESIAN_POINT('Ctrl Pts',(0.897143218189782,1.30632915724249,-0.442820664919227));
#14904=CARTESIAN_POINT('Ctrl Pts',(0.881791875377343,1.3,-0.472691670144998));
#14905=CARTESIAN_POINT('Ctrl Pts',(0.850258932191534,1.3,-0.527308329855002));
#14906=CARTESIAN_POINT('Ctrl Pts',(0.832065554235658,1.30632915724249,-0.555538485325663));
#14907=CARTESIAN_POINT('Ctrl Pts',(0.796153444118959,1.33188468517318,-0.605884303066698));
#14908=CARTESIAN_POINT('Ctrl Pts',(0.778498278845144,1.35110381617461,-0.628048950774009));
#14909=CARTESIAN_POINT('Ctrl Pts',(0.749495710301795,1.39534588636318,-0.662390652284073));
#14910=CARTESIAN_POINT('Ctrl Pts',(0.73619249062986,1.42336732874239,-0.676899590973058));
#14911=CARTESIAN_POINT('Ctrl Pts',(0.718163997970498,1.48491957299737,-0.695997784676727));
#14912=CARTESIAN_POINT('Ctrl Pts',(0.713525491562421,1.5184626473304,-0.700629269222037));
#14913=CARTESIAN_POINT('Ctrl Pts',(0.713525491562421,1.5815373526696,-0.700629269222037));
#14914=CARTESIAN_POINT('Ctrl Pts',(0.718163997970498,1.61508042700263,-0.695997784676727));
#14915=CARTESIAN_POINT('Ctrl Pts',(0.73619249062986,1.67663267125761,-0.676899590973058));
#14916=CARTESIAN_POINT('Ctrl Pts',(0.749495710301795,1.70465411363682,-0.662390652284073));
#14917=CARTESIAN_POINT('Ctrl Pts',(0.778498278845144,1.74889618382539,-0.628048950774009));
#14918=CARTESIAN_POINT('Ctrl Pts',(0.796153444118959,1.76811531482682,-0.605884303066698));
#14919=CARTESIAN_POINT('Ctrl Pts',(0.832065554235658,1.79367084275751,-0.555538485325663));
#14920=CARTESIAN_POINT('Ctrl Pts',(0.850258932191534,1.8,-0.527308329855002));
#14921=CARTESIAN_POINT('Ctrl Pts',(0.881791875377343,1.8,-0.472691670144998));
#14922=CARTESIAN_POINT('Ctrl Pts',(0.897143218189782,1.79367084275751,-0.442820664919227));
#14923=CARTESIAN_POINT('Ctrl Pts',(0.92278792026947,1.76811531482682,-0.386546956384144));
#14924=CARTESIAN_POINT('Ctrl Pts',(0.933155485613026,1.74889618382539,-0.360174810895352));
#14925=CARTESIAN_POINT('Ctrl Pts',(0.948394987258249,1.70465411363682,-0.31788699900678));
#14926=CARTESIAN_POINT('Ctrl Pts',(0.954308486908894,1.67663267125761,-0.299111603474267));
#14927=CARTESIAN_POINT('Ctrl Pts',(0.961833761492987,1.61508042700263,-0.273949373987484));
#14928=CARTESIAN_POINT('Ctrl Pts',(0.963525491562421,1.5815373526696,-0.267616567329817));
#14929=CARTESIAN_POINT('Ctrl Pts',(0.963525491562421,1.55,-0.267616567329817));
#14930=CARTESIAN_POINT('',(0.125,1.55,0.21650635094611));
#14931=CARTESIAN_POINT('Origin',(0.,1.55,0.));
#14932=CARTESIAN_POINT('',(-0.25,1.55,-0.968245836551854));
#14933=CARTESIAN_POINT('',(-0.25,1.55,0.));
#14934=CARTESIAN_POINT('Ctrl Pts',(-0.25,1.55,-0.968245836551854));
#14935=CARTESIAN_POINT('Ctrl Pts',(-0.25,1.5815373526696,-0.968245836551854));
#14936=CARTESIAN_POINT('Ctrl Pts',(-0.243669763522489,1.61508042700263,
-0.969947158664211));
#14937=CARTESIAN_POINT('Ctrl Pts',(-0.218115996279034,1.67663267125761,
-0.976011194447325));
#14938=CARTESIAN_POINT('Ctrl Pts',(-0.198899276956455,1.70465411363682,
-0.980277651290853));
#14939=CARTESIAN_POINT('Ctrl Pts',(-0.154657206767882,1.74889618382539,
-0.988223761669361));
#14940=CARTESIAN_POINT('Ctrl Pts',(-0.126634476150511,1.76811531482682,
-0.992431259450842));
#14941=CARTESIAN_POINT('Ctrl Pts',(-0.0650776639541238,1.79367084275751,
-0.99835915024489));
#14942=CARTESIAN_POINT('Ctrl Pts',(-0.0315329431858092,1.8,-1.));
#14943=CARTESIAN_POINT('Ctrl Pts',(0.0315329431858092,1.8,-1.));
#14944=CARTESIAN_POINT('Ctrl Pts',(0.0650776639541238,1.79367084275751,
-0.99835915024489));
#14945=CARTESIAN_POINT('Ctrl Pts',(0.126634476150511,1.76811531482682,-0.992431259450842));
#14946=CARTESIAN_POINT('Ctrl Pts',(0.154657206767882,1.74889618382539,-0.988223761669361));
#14947=CARTESIAN_POINT('Ctrl Pts',(0.198899276956455,1.70465411363682,-0.980277651290853));
#14948=CARTESIAN_POINT('Ctrl Pts',(0.218115996279034,1.67663267125761,-0.976011194447325));
#14949=CARTESIAN_POINT('Ctrl Pts',(0.243669763522488,1.61508042700263,-0.969947158664211));
#14950=CARTESIAN_POINT('Ctrl Pts',(0.25,1.5815373526696,-0.968245836551854));
#14951=CARTESIAN_POINT('Ctrl Pts',(0.25,1.5184626473304,-0.968245836551854));
#14952=CARTESIAN_POINT('Ctrl Pts',(0.243669763522488,1.48491957299737,-0.969947158664211));
#14953=CARTESIAN_POINT('Ctrl Pts',(0.218115996279034,1.42336732874239,-0.976011194447325));
#14954=CARTESIAN_POINT('Ctrl Pts',(0.198899276956455,1.39534588636318,-0.980277651290853));
#14955=CARTESIAN_POINT('Ctrl Pts',(0.154657206767882,1.35110381617461,-0.988223761669361));
#14956=CARTESIAN_POINT('Ctrl Pts',(0.126634476150511,1.33188468517318,-0.992431259450842));
#14957=CARTESIAN_POINT('Ctrl Pts',(0.0650776639541239,1.30632915724249,
-0.99835915024489));
#14958=CARTESIAN_POINT('Ctrl Pts',(0.0315329431858092,1.3,-1.));
#14959=CARTESIAN_POINT('Ctrl Pts',(-0.0315329431858092,1.3,-1.));
#14960=CARTESIAN_POINT('Ctrl Pts',(-0.0650776639541239,1.30632915724249,
-0.99835915024489));
#14961=CARTESIAN_POINT('Ctrl Pts',(-0.126634476150511,1.33188468517318,
-0.992431259450842));
#14962=CARTESIAN_POINT('Ctrl Pts',(-0.154657206767882,1.35110381617461,
-0.988223761669361));
#14963=CARTESIAN_POINT('Ctrl Pts',(-0.198899276956455,1.39534588636318,
-0.980277651290853));
#14964=CARTESIAN_POINT('Ctrl Pts',(-0.218115996279034,1.42336732874239,
-0.976011194447325));
#14965=CARTESIAN_POINT('Ctrl Pts',(-0.243669763522489,1.48491957299737,
-0.969947158664211));
#14966=CARTESIAN_POINT('Ctrl Pts',(-0.25,1.5184626473304,-0.968245836551854));
#14967=CARTESIAN_POINT('Ctrl Pts',(-0.25,1.55,-0.968245836551854));
#14968=CARTESIAN_POINT('Origin',(0.,1.55,0.));
#14969=CARTESIAN_POINT('',(-0.25,1.55,0.968245836551854));
#14970=CARTESIAN_POINT('Ctrl Pts',(-0.25,1.55,0.968245836551854));
#14971=CARTESIAN_POINT('Ctrl Pts',(-0.25,1.5184626473304,0.968245836551854));
#14972=CARTESIAN_POINT('Ctrl Pts',(-0.243669763522489,1.48491957299737,
0.969947158664211));
#14973=CARTESIAN_POINT('Ctrl Pts',(-0.218115996279034,1.42336732874239,
0.976011194447325));
#14974=CARTESIAN_POINT('Ctrl Pts',(-0.198899276956455,1.39534588636318,
0.980277651290853));
#14975=CARTESIAN_POINT('Ctrl Pts',(-0.154657206767882,1.35110381617461,
0.988223761669361));
#14976=CARTESIAN_POINT('Ctrl Pts',(-0.126634476150511,1.33188468517318,
0.992431259450842));
#14977=CARTESIAN_POINT('Ctrl Pts',(-0.065077663954124,1.30632915724249,
0.99835915024489));
#14978=CARTESIAN_POINT('Ctrl Pts',(-0.0315329431858092,1.3,1.));
#14979=CARTESIAN_POINT('Ctrl Pts',(0.0315329431858092,1.3,1.));
#14980=CARTESIAN_POINT('Ctrl Pts',(0.065077663954124,1.30632915724249,0.99835915024489));
#14981=CARTESIAN_POINT('Ctrl Pts',(0.126634476150511,1.33188468517318,0.992431259450842));
#14982=CARTESIAN_POINT('Ctrl Pts',(0.154657206767882,1.35110381617461,0.988223761669361));
#14983=CARTESIAN_POINT('Ctrl Pts',(0.198899276956455,1.39534588636318,0.980277651290853));
#14984=CARTESIAN_POINT('Ctrl Pts',(0.218115996279034,1.42336732874239,0.976011194447325));
#14985=CARTESIAN_POINT('Ctrl Pts',(0.243669763522488,1.48491957299737,0.969947158664211));
#14986=CARTESIAN_POINT('Ctrl Pts',(0.25,1.5184626473304,0.968245836551854));
#14987=CARTESIAN_POINT('Ctrl Pts',(0.25,1.5815373526696,0.968245836551854));
#14988=CARTESIAN_POINT('Ctrl Pts',(0.243669763522488,1.61508042700263,0.969947158664211));
#14989=CARTESIAN_POINT('Ctrl Pts',(0.218115996279034,1.67663267125761,0.976011194447325));
#14990=CARTESIAN_POINT('Ctrl Pts',(0.198899276956455,1.70465411363682,0.980277651290853));
#14991=CARTESIAN_POINT('Ctrl Pts',(0.154657206767882,1.74889618382539,0.988223761669361));
#14992=CARTESIAN_POINT('Ctrl Pts',(0.126634476150511,1.76811531482682,0.992431259450842));
#14993=CARTESIAN_POINT('Ctrl Pts',(0.0650776639541239,1.79367084275751,
0.99835915024489));
#14994=CARTESIAN_POINT('Ctrl Pts',(0.0315329431858092,1.8,1.));
#14995=CARTESIAN_POINT('Ctrl Pts',(-0.0315329431858092,1.8,1.));
#14996=CARTESIAN_POINT('Ctrl Pts',(-0.0650776639541239,1.79367084275751,
0.99835915024489));
#14997=CARTESIAN_POINT('Ctrl Pts',(-0.126634476150511,1.76811531482682,
0.992431259450842));
#14998=CARTESIAN_POINT('Ctrl Pts',(-0.154657206767882,1.74889618382539,
0.988223761669361));
#14999=CARTESIAN_POINT('Ctrl Pts',(-0.198899276956455,1.70465411363682,
0.980277651290853));
#15000=CARTESIAN_POINT('Ctrl Pts',(-0.218115996279034,1.67663267125761,
0.976011194447325));
#15001=CARTESIAN_POINT('Ctrl Pts',(-0.243669763522489,1.61508042700263,
0.969947158664211));
#15002=CARTESIAN_POINT('Ctrl Pts',(-0.25,1.5815373526696,0.968245836551854));
#15003=CARTESIAN_POINT('Ctrl Pts',(-0.25,1.55,0.968245836551854));
#15004=CARTESIAN_POINT('',(-0.25,1.55,0.));
#15005=CARTESIAN_POINT('Origin',(1.65,2.25,0.));
#15006=CARTESIAN_POINT('',(-1.,2.25,-1.22464679914735E-16));
#15007=CARTESIAN_POINT('Origin',(0.,2.25,0.));
#15008=CARTESIAN_POINT('Origin',(1.75,0.85,0.));
#15009=CARTESIAN_POINT('',(-1.75,0.85,-2.14313189850787E-16));
#15010=CARTESIAN_POINT('Origin',(0.,0.85,0.));
#15011=CARTESIAN_POINT('Origin',(0.,0.,0.));
#15012=CARTESIAN_POINT('',(-1.75,-0.85,-2.14313189850787E-16));
#15013=CARTESIAN_POINT('Origin',(0.,-0.85,0.));
#15014=CARTESIAN_POINT('',(-1.75,0.,-2.14313189850787E-16));
#15015=CARTESIAN_POINT('Origin',(1.,-0.85,0.));
#15016=CARTESIAN_POINT('',(-1.,-0.85,-1.22464679914735E-16));
#15017=CARTESIAN_POINT('Origin',(0.,-0.85,0.));
#15018=CARTESIAN_POINT('Origin',(0.,0.7,0.));
#15019=CARTESIAN_POINT('',(-1.,0.7,-1.22464679914735E-16));
#15020=CARTESIAN_POINT('',(0.,0.,0.));
#15021=CARTESIAN_POINT('',(0.,0.,0.));
#15022=CARTESIAN_POINT('',(0.,0.,0.));
#15023=CARTESIAN_POINT('Origin',(0.,0.,0.));
#15024=CARTESIAN_POINT('',(-0.42,0.16,5.14351655641888E-17));
#15025=CARTESIAN_POINT('Origin',(0.,0.16,0.));
#15026=CARTESIAN_POINT('',(-0.42,0.,5.14351655641888E-17));
#15027=CARTESIAN_POINT('',(-0.42,0.,5.14351655641888E-17));
#15028=CARTESIAN_POINT('Origin',(0.,0.,0.));
#15029=CARTESIAN_POINT('Origin',(0.,0.,0.));
#15030=CARTESIAN_POINT('',(-0.8,0.16,9.79717439317883E-17));
#15031=CARTESIAN_POINT('Origin',(0.,0.16,0.));
#15032=CARTESIAN_POINT('',(-0.8,0.,9.79717439317883E-17));
#15033=CARTESIAN_POINT('',(-0.8,0.,9.79717439317883E-17));
#15034=CARTESIAN_POINT('Origin',(0.,0.,0.));
#15035=CARTESIAN_POINT('Origin',(0.,0.16,0.));
#15036=CARTESIAN_POINT('Origin',(0.,0.,0.));
#15037=CARTESIAN_POINT('',(0.,0.,0.));
#15038=CARTESIAN_POINT('Origin',(0.173205080756888,-0.8,-0.3));
#15039=CARTESIAN_POINT('',(0.346410161513775,-0.8,0.));
#15040=CARTESIAN_POINT('',(0.173205080756888,-0.8,-0.3));
#15041=CARTESIAN_POINT('',(0.346410161513775,-0.8,0.));
#15042=CARTESIAN_POINT('',(0.173205080756888,-1.28,-0.3));
#15043=CARTESIAN_POINT('',(0.173205080756888,-0.8,-0.3));
#15044=CARTESIAN_POINT('',(0.346410161513775,-1.28,0.));
#15045=CARTESIAN_POINT('',(0.346410161513775,-1.28,0.));
#15046=CARTESIAN_POINT('',(0.346410161513775,-0.8,0.));
#15047=CARTESIAN_POINT('Origin',(-0.173205080756888,-0.8,-0.3));
#15048=CARTESIAN_POINT('',(-0.173205080756888,-0.8,-0.3));
#15049=CARTESIAN_POINT('',(0.173205080756888,-0.8,-0.3));
#15050=CARTESIAN_POINT('',(-0.173205080756888,-1.28,-0.3));
#15051=CARTESIAN_POINT('',(-0.173205080756888,-0.8,-0.3));
#15052=CARTESIAN_POINT('',(0.173205080756888,-1.28,-0.3));
#15053=CARTESIAN_POINT('Origin',(-0.346410161513775,-0.8,-5.55111512312578E-17));
#15054=CARTESIAN_POINT('',(-0.346410161513775,-0.8,-4.24230095489963E-17));
#15055=CARTESIAN_POINT('',(-0.173205080756888,-0.8,-0.3));
#15056=CARTESIAN_POINT('',(-0.346410161513775,-1.28,-5.55111512312578E-17));
#15057=CARTESIAN_POINT('',(-0.346410161513775,-0.8,-4.24230095489963E-17));
#15058=CARTESIAN_POINT('',(-0.173205080756888,-1.28,-0.3));
#15059=CARTESIAN_POINT('Origin',(-0.173205080756888,-0.8,0.3));
#15060=CARTESIAN_POINT('',(-0.173205080756888,-0.8,0.3));
#15061=CARTESIAN_POINT('',(-0.346410161513775,-0.8,-4.24230095489963E-17));
#15062=CARTESIAN_POINT('',(-0.173205080756888,-1.28,0.3));
#15063=CARTESIAN_POINT('',(-0.173205080756888,-0.8,0.3));
#15064=CARTESIAN_POINT('',(-0.346410161513775,-1.28,-4.24230095489963E-17));
#15065=CARTESIAN_POINT('Origin',(0.173205080756888,-0.8,0.3));
#15066=CARTESIAN_POINT('',(0.173205080756888,-0.8,0.3));
#15067=CARTESIAN_POINT('',(-0.173205080756888,-0.8,0.3));
#15068=CARTESIAN_POINT('',(0.173205080756888,-1.28,0.3));
#15069=CARTESIAN_POINT('',(0.173205080756888,-0.8,0.3));
#15070=CARTESIAN_POINT('',(-0.173205080756888,-1.28,0.3));
#15071=CARTESIAN_POINT('Origin',(0.346410161513775,-0.8,0.));
#15072=CARTESIAN_POINT('',(0.173205080756888,-0.8,0.3));
#15073=CARTESIAN_POINT('',(0.173205080756888,-1.28,0.3));
#15074=CARTESIAN_POINT('Origin',(0.,-0.8,-5.55111512312578E-17));
#15075=CARTESIAN_POINT('Origin',(0.,-1.28,-5.55111512312578E-17));
#15076=CARTESIAN_POINT('Origin',(0.,-2.5,0.));
#15077=CARTESIAN_POINT('',(-0.3933,-2.5,4.81653586104654E-17));
#15078=CARTESIAN_POINT('Origin',(0.,-2.5,0.));
#15079=CARTESIAN_POINT('Origin',(0.6,0.8,0.));
#15080=CARTESIAN_POINT('',(-0.6,0.8,-7.34788079488412E-17));
#15081=CARTESIAN_POINT('Origin',(0.,0.8,0.));
#15082=CARTESIAN_POINT('Origin',(0.,0.775,0.));
#15083=CARTESIAN_POINT('',(-0.65,0.75,-7.9602041944578E-17));
#15084=CARTESIAN_POINT('Origin',(0.,0.75,0.));
#15085=CARTESIAN_POINT('',(-0.625,0.775,-7.65404249467096E-17));
#15086=CARTESIAN_POINT('Origin',(0.,0.39,0.));
#15087=CARTESIAN_POINT('',(-0.65,0.0299999999999998,-7.9602041944578E-17));
#15088=CARTESIAN_POINT('Origin',(0.,0.0299999999999998,0.));
#15089=CARTESIAN_POINT('',(-0.65,0.39,-7.9602041944578E-17));
#15090=CARTESIAN_POINT('Origin',(0.,0.0150000000000001,0.));
#15091=CARTESIAN_POINT('',(-0.62,5.89805981832114E-17,-7.59281015471359E-17));
#15092=CARTESIAN_POINT('Origin',(0.,0.,0.));
#15093=CARTESIAN_POINT('',(-0.635,0.0150000000000001,-7.77650717458569E-17));
#15094=CARTESIAN_POINT('Origin',(0.42,0.,0.));
#15095=CARTESIAN_POINT('',(-0.42,-3.46944695195361E-18,-5.14351655641888E-17));
#15096=CARTESIAN_POINT('Origin',(0.,0.,0.));
#15097=CARTESIAN_POINT('Origin',(0.,-0.02,0.));
#15098=CARTESIAN_POINT('',(-0.3933,-0.0534000000000001,4.81653586104654E-17));
#15099=CARTESIAN_POINT('Origin',(0.,-0.0534000000000001,0.));
#15100=CARTESIAN_POINT('',(-0.41,-0.02,-5.02105187650415E-17));
#15101=CARTESIAN_POINT('Origin',(0.,-1.48,0.));
#15102=CARTESIAN_POINT('',(-0.3933,-1.48,-4.81653586104654E-17));
#15103=CARTESIAN_POINT('',(0.,0.,0.));
#15104=CARTESIAN_POINT('Origin',(-1.6,0.,1.3));
#15105=CARTESIAN_POINT('',(-1.2,0.340036762718386,1.3));
#15106=CARTESIAN_POINT('',(-1.2,-0.340036762718386,1.3));
#15107=CARTESIAN_POINT('',(-1.2,0.,1.3));
#15108=CARTESIAN_POINT('Origin',(-1.6,0.,1.3));
#15109=CARTESIAN_POINT('Origin',(-1.6,0.,0.6));
#15110=CARTESIAN_POINT('',(-1.2,0.340036762718386,0.6));
#15111=CARTESIAN_POINT('',(-1.2,0.340036762718386,0.6));
#15112=CARTESIAN_POINT('',(-1.2,-0.340036762718386,0.6));
#15113=CARTESIAN_POINT('Origin',(-1.6,0.,0.6));
#15114=CARTESIAN_POINT('',(-1.2,-0.340036762718386,0.6));
#15115=CARTESIAN_POINT('Origin',(1.6,0.,0.6));
#15116=CARTESIAN_POINT('',(1.2,0.340036762718386,1.3));
#15117=CARTESIAN_POINT('',(1.2,0.340036762718386,0.6));
#15118=CARTESIAN_POINT('',(1.2,0.340036762718386,0.6));
#15119=CARTESIAN_POINT('',(1.2,-0.340036762718386,1.3));
#15120=CARTESIAN_POINT('Origin',(1.6,0.,1.3));
#15121=CARTESIAN_POINT('',(1.2,-0.340036762718386,0.6));
#15122=CARTESIAN_POINT('',(1.2,-0.340036762718386,0.6));
#15123=CARTESIAN_POINT('Origin',(1.6,0.,0.6));
#15124=CARTESIAN_POINT('Origin',(1.6,0.,1.3));
#15125=CARTESIAN_POINT('',(1.2,0.,1.3));
#15126=CARTESIAN_POINT('Origin',(-2.1,0.,0.6));
#15127=CARTESIAN_POINT('',(-1.2,0.7,0.6));
#15128=CARTESIAN_POINT('',(-1.2,0.,0.6));
#15129=CARTESIAN_POINT('',(-2.1,0.7,0.6));
#15130=CARTESIAN_POINT('',(-1.2,0.7,0.6));
#15131=CARTESIAN_POINT('',(-2.1,-0.7,0.6));
#15132=CARTESIAN_POINT('',(-2.1,0.,0.6));
#15133=CARTESIAN_POINT('',(-1.2,-0.7,0.6));
#15134=CARTESIAN_POINT('',(-1.2,-0.7,0.6));
#15135=CARTESIAN_POINT('',(-1.2,0.,0.6));
#15136=CARTESIAN_POINT('',(-1.875,3.36777869765522E-17,0.6));
#15137=CARTESIAN_POINT('Origin',(-1.6,0.,0.6));
#15138=CARTESIAN_POINT('Origin',(-1.2,0.,0.6));
#15139=CARTESIAN_POINT('',(-1.2,-0.7,3.75));
#15140=CARTESIAN_POINT('',(-1.2,-0.7,3.75));
#15141=CARTESIAN_POINT('',(-1.2,0.7,3.75));
#15142=CARTESIAN_POINT('',(-1.2,0.,3.75));
#15143=CARTESIAN_POINT('',(-1.2,0.7,3.75));
#15144=CARTESIAN_POINT('',(-1.2,-2.02066721859313E-17,3.515));
#15145=CARTESIAN_POINT('Origin',(-1.2,0.,3.35));
#15146=CARTESIAN_POINT('Origin',(1.2,0.,0.6));
#15147=CARTESIAN_POINT('',(2.1,-0.7,0.6));
#15148=CARTESIAN_POINT('',(2.1,0.7,0.6));
#15149=CARTESIAN_POINT('',(2.1,0.,0.6));
#15150=CARTESIAN_POINT('',(1.2,0.7,0.6));
#15151=CARTESIAN_POINT('',(2.1,0.7,0.6));
#15152=CARTESIAN_POINT('',(1.2,0.,0.6));
#15153=CARTESIAN_POINT('',(1.2,-0.7,0.6));
#15154=CARTESIAN_POINT('',(1.2,0.,0.6));
#15155=CARTESIAN_POINT('',(2.1,-0.7,0.6));
#15156=CARTESIAN_POINT('',(1.325,3.36777869765522E-17,0.6));
#15157=CARTESIAN_POINT('Origin',(1.6,0.,0.6));
#15158=CARTESIAN_POINT('Origin',(0.1,0.,3.35));
#15159=CARTESIAN_POINT('',(0.1,-2.75545529808155E-17,3.575));
#15160=CARTESIAN_POINT('Origin',(0.1,0.,3.35));
#15161=CARTESIAN_POINT('',(1.2,2.75545529808155E-17,3.575));
#15162=CARTESIAN_POINT('',(0.1,-2.75545529808155E-17,3.575));
#15163=CARTESIAN_POINT('Origin',(1.2,0.,3.35));
#15164=CARTESIAN_POINT('Origin',(0.,0.,3.35));
#15165=CARTESIAN_POINT('',(-0.1,2.02066721859313E-17,3.515));
#15166=CARTESIAN_POINT('',(0.,-2.02066721859313E-17,3.515));
#15167=CARTESIAN_POINT('Origin',(-0.1,0.,3.35));
#15168=CARTESIAN_POINT('Origin',(-1.6,0.,-0.05));
#15169=CARTESIAN_POINT('',(-1.875,-3.36777869765522E-17,0.));
#15170=CARTESIAN_POINT('Origin',(-1.6,0.,0.));
#15171=CARTESIAN_POINT('',(-1.875,-3.36777869765522E-17,-0.05));
#15172=CARTESIAN_POINT('Origin',(1.6,0.,-0.05));
#15173=CARTESIAN_POINT('',(1.325,-3.36777869765522E-17,0.));
#15174=CARTESIAN_POINT('Origin',(1.6,0.,0.));
#15175=CARTESIAN_POINT('',(1.325,-3.36777869765522E-17,-0.05));
#15176=CARTESIAN_POINT('Origin',(0.,0.,2.3));
#15177=CARTESIAN_POINT('',(-0.6,-0.7,2.3));
#15178=CARTESIAN_POINT('Origin',(0.,-0.7,2.3));
#15179=CARTESIAN_POINT('',(-0.6,0.7,2.3));
#15180=CARTESIAN_POINT('',(-0.6,0.,2.3));
#15181=CARTESIAN_POINT('Origin',(0.,0.7,2.3));
#15182=CARTESIAN_POINT('Origin',(0.,-0.7,1.875));
#15183=CARTESIAN_POINT('',(-2.1,-0.7,0.));
#15184=CARTESIAN_POINT('',(-2.1,-0.7,0.6));
#15185=CARTESIAN_POINT('',(2.1,-0.7,0.));
#15186=CARTESIAN_POINT('',(-2.1,-0.7,0.));
#15187=CARTESIAN_POINT('',(2.1,-0.7,0.));
#15188=CARTESIAN_POINT('',(1.2,-0.7,3.75));
#15189=CARTESIAN_POINT('',(1.2,-0.7,0.6));
#15190=CARTESIAN_POINT('',(0.1,-0.7,3.75));
#15191=CARTESIAN_POINT('',(1.2,-0.7,3.75));
#15192=CARTESIAN_POINT('',(0.1,-0.7,2.95));
#15193=CARTESIAN_POINT('',(0.1,-0.7,3.75));
#15194=CARTESIAN_POINT('',(-0.1,-0.7,2.95));
#15195=CARTESIAN_POINT('',(0.1,-0.7,2.95));
#15196=CARTESIAN_POINT('',(-0.1,-0.7,3.75));
#15197=CARTESIAN_POINT('',(-0.1,-0.7,2.95));
#15198=CARTESIAN_POINT('',(-0.1,-0.7,3.75));
#15199=CARTESIAN_POINT('Origin',(-2.1,0.,0.));
#15200=CARTESIAN_POINT('',(-2.1,0.7,0.));
#15201=CARTESIAN_POINT('',(-2.1,0.7,0.6));
#15202=CARTESIAN_POINT('',(-2.1,0.,0.));
#15203=CARTESIAN_POINT('Origin',(2.1,0.,0.));
#15204=CARTESIAN_POINT('',(2.1,0.7,0.));
#15205=CARTESIAN_POINT('',(-2.1,0.7,0.));
#15206=CARTESIAN_POINT('',(2.1,0.,0.));
#15207=CARTESIAN_POINT('Origin',(2.1,0.,0.6));
#15208=CARTESIAN_POINT('',(2.1,0.7,0.));
#15209=CARTESIAN_POINT('Origin',(1.2,0.,3.75));
#15210=CARTESIAN_POINT('',(1.2,0.7,3.75));
#15211=CARTESIAN_POINT('',(1.2,0.7,0.6));
#15212=CARTESIAN_POINT('',(1.2,0.,3.75));
#15213=CARTESIAN_POINT('Origin',(0.1,0.,3.75));
#15214=CARTESIAN_POINT('',(0.1,0.7,3.75));
#15215=CARTESIAN_POINT('',(1.2,0.7,3.75));
#15216=CARTESIAN_POINT('',(0.1,0.,3.75));
#15217=CARTESIAN_POINT('Origin',(0.1,0.,2.95));
#15218=CARTESIAN_POINT('',(0.1,0.7,2.95));
#15219=CARTESIAN_POINT('',(0.1,0.7,3.75));
#15220=CARTESIAN_POINT('',(0.1,0.,2.95));
#15221=CARTESIAN_POINT('Origin',(-0.1,0.,2.95));
#15222=CARTESIAN_POINT('',(-0.1,0.7,2.95));
#15223=CARTESIAN_POINT('',(0.1,0.7,2.95));
#15224=CARTESIAN_POINT('',(-0.1,0.,2.95));
#15225=CARTESIAN_POINT('Origin',(-0.1,0.,3.75));
#15226=CARTESIAN_POINT('',(-0.1,0.7,3.75));
#15227=CARTESIAN_POINT('',(-0.1,0.7,2.95));
#15228=CARTESIAN_POINT('',(-0.1,0.,3.75));
#15229=CARTESIAN_POINT('Origin',(-1.2,0.,3.75));
#15230=CARTESIAN_POINT('',(-0.1,0.7,3.75));
#15231=CARTESIAN_POINT('Origin',(0.,0.7,1.875));
#15232=CARTESIAN_POINT('',(0.,0.,0.));
#15233=CARTESIAN_POINT('Origin',(0.,0.09,0.));
#15234=CARTESIAN_POINT('',(-0.285,0.1,3.49024337756996E-17));
#15235=CARTESIAN_POINT('Origin',(0.,0.1,0.));
#15236=CARTESIAN_POINT('',(-0.265,0.08,-3.24531401774049E-17));
#15237=CARTESIAN_POINT('',(-0.275,0.09,3.36777869765522E-17));
#15238=CARTESIAN_POINT('Origin',(0.,0.08,0.));
#15239=CARTESIAN_POINT('Origin',(0.,0.,0.));
#15240=CARTESIAN_POINT('',(-0.265,0.,3.24531401774049E-17));
#15241=CARTESIAN_POINT('',(-0.265,0.,3.24531401774049E-17));
#15242=CARTESIAN_POINT('Origin',(0.,0.,0.));
#15243=CARTESIAN_POINT('Origin',(0.,0.1,0.));
#15244=CARTESIAN_POINT('',(-0.5,0.1,6.12323399573677E-17));
#15245=CARTESIAN_POINT('Origin',(0.,0.1,0.));
#15246=CARTESIAN_POINT('Origin',(0.,0.,0.));
#15247=CARTESIAN_POINT('',(-0.5,0.,6.12323399573677E-17));
#15248=CARTESIAN_POINT('',(-0.5,0.,6.12323399573677E-17));
#15249=CARTESIAN_POINT('Origin',(0.,0.,0.));
#15250=CARTESIAN_POINT('Origin',(0.,0.,0.));
#15251=CARTESIAN_POINT('',(0.,0.,0.));
#15252=CARTESIAN_POINT('Origin',(0.115470053837925,-0.5,-0.2));
#15253=CARTESIAN_POINT('',(0.23094010767585,-0.5,0.));
#15254=CARTESIAN_POINT('',(0.115470053837925,-0.5,-0.2));
#15255=CARTESIAN_POINT('',(0.23094010767585,-0.5,0.));
#15256=CARTESIAN_POINT('',(0.115470053837925,-0.8,-0.2));
#15257=CARTESIAN_POINT('',(0.115470053837925,-0.5,-0.2));
#15258=CARTESIAN_POINT('',(0.23094010767585,-0.8,0.));
#15259=CARTESIAN_POINT('',(0.23094010767585,-0.8,0.));
#15260=CARTESIAN_POINT('',(0.23094010767585,-0.5,0.));
#15261=CARTESIAN_POINT('Origin',(-0.115470053837925,-0.5,-0.2));
#15262=CARTESIAN_POINT('',(-0.115470053837925,-0.5,-0.2));
#15263=CARTESIAN_POINT('',(0.115470053837925,-0.5,-0.2));
#15264=CARTESIAN_POINT('',(-0.115470053837925,-0.8,-0.2));
#15265=CARTESIAN_POINT('',(-0.115470053837925,-0.5,-0.2));
#15266=CARTESIAN_POINT('',(0.115470053837925,-0.8,-0.2));
#15267=CARTESIAN_POINT('Origin',(-0.23094010767585,-0.5,-2.77555756156289E-17));
#15268=CARTESIAN_POINT('',(-0.23094010767585,-0.5,-2.82820063659975E-17));
#15269=CARTESIAN_POINT('',(-0.115470053837925,-0.5,-0.2));
#15270=CARTESIAN_POINT('',(-0.23094010767585,-0.8,-2.77555756156289E-17));
#15271=CARTESIAN_POINT('',(-0.23094010767585,-0.5,-2.82820063659975E-17));
#15272=CARTESIAN_POINT('',(-0.115470053837925,-0.8,-0.2));
#15273=CARTESIAN_POINT('Origin',(-0.115470053837925,-0.5,0.2));
#15274=CARTESIAN_POINT('',(-0.115470053837925,-0.5,0.2));
#15275=CARTESIAN_POINT('',(-0.23094010767585,-0.5,-2.82820063659975E-17));
#15276=CARTESIAN_POINT('',(-0.115470053837925,-0.8,0.2));
#15277=CARTESIAN_POINT('',(-0.115470053837925,-0.5,0.2));
#15278=CARTESIAN_POINT('',(-0.23094010767585,-0.8,-2.82820063659975E-17));
#15279=CARTESIAN_POINT('Origin',(0.115470053837925,-0.5,0.2));
#15280=CARTESIAN_POINT('',(0.115470053837925,-0.5,0.2));
#15281=CARTESIAN_POINT('',(-0.115470053837925,-0.5,0.2));
#15282=CARTESIAN_POINT('',(0.115470053837925,-0.8,0.2));
#15283=CARTESIAN_POINT('',(0.115470053837925,-0.5,0.2));
#15284=CARTESIAN_POINT('',(-0.115470053837925,-0.8,0.2));
#15285=CARTESIAN_POINT('Origin',(0.23094010767585,-0.5,0.));
#15286=CARTESIAN_POINT('',(0.115470053837925,-0.5,0.2));
#15287=CARTESIAN_POINT('',(0.115470053837925,-0.8,0.2));
#15288=CARTESIAN_POINT('Origin',(0.,-0.5,0.));
#15289=CARTESIAN_POINT('Origin',(0.,-0.8,0.));
#15290=CARTESIAN_POINT('Origin',(0.,-1.4,0.));
#15291=CARTESIAN_POINT('',(-0.24505,-1.4,3.00099698131059E-17));
#15292=CARTESIAN_POINT('Origin',(0.,-1.4,0.));
#15293=CARTESIAN_POINT('Origin',(0.375,0.5,0.));
#15294=CARTESIAN_POINT('',(-0.375,0.5,-4.59242549680257E-17));
#15295=CARTESIAN_POINT('Origin',(0.,0.5,0.));
#15296=CARTESIAN_POINT('Origin',(0.,0.475,0.));
#15297=CARTESIAN_POINT('',(-0.425,0.45,-5.20474889637625E-17));
#15298=CARTESIAN_POINT('Origin',(0.,0.45,0.));
#15299=CARTESIAN_POINT('',(-0.4,0.475,-4.89858719658941E-17));
#15300=CARTESIAN_POINT('Origin',(0.,0.24,0.));
#15301=CARTESIAN_POINT('',(-0.425,0.0299999999999998,-5.20474889637625E-17));
#15302=CARTESIAN_POINT('Origin',(0.,0.0299999999999998,0.));
#15303=CARTESIAN_POINT('',(-0.425,0.24,-5.20474889637625E-17));
#15304=CARTESIAN_POINT('Origin',(0.,0.0150000000000001,0.));
#15305=CARTESIAN_POINT('',(-0.395,4.85722573273506E-17,-4.83735485663204E-17));
#15306=CARTESIAN_POINT('Origin',(0.,0.,0.));
#15307=CARTESIAN_POINT('',(-0.41,0.0150000000000001,-5.02105187650415E-17));
#15308=CARTESIAN_POINT('Origin',(0.27,0.,0.));
#15309=CARTESIAN_POINT('',(-0.27,0.,-3.30654635769785E-17));
#15310=CARTESIAN_POINT('Origin',(0.,0.,0.));
#15311=CARTESIAN_POINT('Origin',(0.,-0.02,0.));
#15312=CARTESIAN_POINT('',(-0.24505,-0.0498999999999999,3.00099698131059E-17));
#15313=CARTESIAN_POINT('Origin',(0.,-0.0498999999999999,0.));
#15314=CARTESIAN_POINT('',(-0.26,-0.02,-3.18408167778312E-17));
#15315=CARTESIAN_POINT('Origin',(0.,-0.995,0.));
#15316=CARTESIAN_POINT('',(-0.24505,-0.995,-3.00099698131059E-17));
#15317=CARTESIAN_POINT('',(0.,0.,0.));
#15318=CARTESIAN_POINT('Origin',(0.3,0.4,0.));
#15319=CARTESIAN_POINT('',(-0.3,0.4,-3.67394039744206E-17));
#15320=CARTESIAN_POINT('Origin',(0.,0.4,0.));
#15321=CARTESIAN_POINT('Origin',(0.,0.375,0.));
#15322=CARTESIAN_POINT('',(-0.35,0.35,-4.28626379701573E-17));
#15323=CARTESIAN_POINT('Origin',(0.,0.35,0.));
#15324=CARTESIAN_POINT('',(-0.325,0.375,-3.9801020972289E-17));
#15325=CARTESIAN_POINT('Origin',(0.,0.19,0.));
#15326=CARTESIAN_POINT('',(-0.35,0.03,-4.28626379701574E-17));
#15327=CARTESIAN_POINT('Origin',(0.,0.03,0.));
#15328=CARTESIAN_POINT('',(-0.35,0.19,-4.28626379701574E-17));
#15329=CARTESIAN_POINT('Origin',(0.,0.0149999999999999,0.));
#15330=CARTESIAN_POINT('',(-0.32,-3.29597460435593E-17,-3.91886975727153E-17));
#15331=CARTESIAN_POINT('Origin',(0.,0.,0.));
#15332=CARTESIAN_POINT('',(-0.335,0.0149999999999999,-4.10256677714363E-17));
#15333=CARTESIAN_POINT('Origin',(0.22,0.,0.));
#15334=CARTESIAN_POINT('',(-0.22,-6.93889390390723E-18,-2.69422295812418E-17));
#15335=CARTESIAN_POINT('Origin',(0.,0.,0.));
#15336=CARTESIAN_POINT('Origin',(0.,-0.02,0.));
#15337=CARTESIAN_POINT('',(-0.1954,-0.0492,2.39295984553393E-17));
#15338=CARTESIAN_POINT('Origin',(0.,-0.0492,0.));
#15339=CARTESIAN_POINT('',(-0.21,-0.02,-2.57175827820944E-17));
#15340=CARTESIAN_POINT('Origin',(0.,-0.8,0.));
#15341=CARTESIAN_POINT('',(-0.1954,-1.5646,2.39295984553393E-17));
#15342=CARTESIAN_POINT('Origin',(0.,-1.5646,0.));
#15343=CARTESIAN_POINT('',(-0.1954,-0.8,-2.39295984553393E-17));
#15344=CARTESIAN_POINT('Origin',(0.,-1.58,0.));
#15345=CARTESIAN_POINT('',(-0.16,-1.6,-1.95943487863577E-17));
#15346=CARTESIAN_POINT('Origin',(0.,-1.6,0.));
#15347=CARTESIAN_POINT('',(-0.18,-1.58,-2.20436423846524E-17));
#15348=CARTESIAN_POINT('Origin',(0.,-1.6,0.));
#15349=CARTESIAN_POINT('Origin',(0.0866025403784439,-0.4,-0.15));
#15350=CARTESIAN_POINT('',(0.173205080756888,-0.4,0.));
#15351=CARTESIAN_POINT('',(0.0866025403784439,-0.4,-0.15));
#15352=CARTESIAN_POINT('',(0.173205080756888,-0.4,0.));
#15353=CARTESIAN_POINT('',(0.0866025403784439,-0.64,-0.15));
#15354=CARTESIAN_POINT('',(0.0866025403784439,-0.4,-0.15));
#15355=CARTESIAN_POINT('',(0.173205080756888,-0.64,0.));
#15356=CARTESIAN_POINT('',(0.173205080756888,-0.64,0.));
#15357=CARTESIAN_POINT('',(0.173205080756888,-0.4,0.));
#15358=CARTESIAN_POINT('Origin',(-0.0866025403784438,-0.4,-0.15));
#15359=CARTESIAN_POINT('',(-0.0866025403784438,-0.4,-0.15));
#15360=CARTESIAN_POINT('',(0.0866025403784439,-0.4,-0.15));
#15361=CARTESIAN_POINT('',(-0.0866025403784438,-0.64,-0.15));
#15362=CARTESIAN_POINT('',(-0.0866025403784438,-0.4,-0.15));
#15363=CARTESIAN_POINT('',(0.0866025403784439,-0.64,-0.15));
#15364=CARTESIAN_POINT('Origin',(-0.173205080756888,-0.4,-2.77555756156289E-17));
#15365=CARTESIAN_POINT('',(-0.173205080756888,-0.4,-2.12115047744981E-17));
#15366=CARTESIAN_POINT('',(-0.0866025403784438,-0.4,-0.15));
#15367=CARTESIAN_POINT('',(-0.173205080756888,-0.64,-2.77555756156289E-17));
#15368=CARTESIAN_POINT('',(-0.173205080756888,-0.4,-2.12115047744981E-17));
#15369=CARTESIAN_POINT('',(-0.0866025403784438,-0.64,-0.15));
#15370=CARTESIAN_POINT('Origin',(-0.0866025403784439,-0.4,0.15));
#15371=CARTESIAN_POINT('',(-0.0866025403784439,-0.4,0.15));
#15372=CARTESIAN_POINT('',(-0.173205080756888,-0.4,-2.12115047744981E-17));
#15373=CARTESIAN_POINT('',(-0.0866025403784439,-0.64,0.15));
#15374=CARTESIAN_POINT('',(-0.0866025403784439,-0.4,0.15));
#15375=CARTESIAN_POINT('',(-0.173205080756888,-0.64,-2.12115047744981E-17));
#15376=CARTESIAN_POINT('Origin',(0.0866025403784439,-0.4,0.15));
#15377=CARTESIAN_POINT('',(0.0866025403784439,-0.4,0.15));
#15378=CARTESIAN_POINT('',(-0.0866025403784439,-0.4,0.15));
#15379=CARTESIAN_POINT('',(0.0866025403784439,-0.64,0.15));
#15380=CARTESIAN_POINT('',(0.0866025403784439,-0.4,0.15));
#15381=CARTESIAN_POINT('',(-0.0866025403784439,-0.64,0.15));
#15382=CARTESIAN_POINT('Origin',(0.173205080756888,-0.4,0.));
#15383=CARTESIAN_POINT('',(0.0866025403784439,-0.4,0.15));
#15384=CARTESIAN_POINT('',(0.0866025403784439,-0.64,0.15));
#15385=CARTESIAN_POINT('Origin',(0.,-0.4,-2.77555756156289E-17));
#15386=CARTESIAN_POINT('Origin',(0.,-0.64,-2.77555756156289E-17));
#15387=CARTESIAN_POINT('',(0.,0.,0.));
#15388=CARTESIAN_POINT('Origin',(20.,0.,0.));
#15389=CARTESIAN_POINT('',(20.,7.34788079488412E-17,0.6));
#15390=CARTESIAN_POINT('Origin',(20.,0.,0.));
#15391=CARTESIAN_POINT('Origin',(0.05,0.,0.));
#15392=CARTESIAN_POINT('',(0.1,7.34788079488412E-17,0.6));
#15393=CARTESIAN_POINT('Origin',(0.1,0.,0.));
#15394=CARTESIAN_POINT('',(0.,-6.12323399573677E-17,0.5));
#15395=CARTESIAN_POINT('',(0.05,-6.73555739531044E-17,0.55));
#15396=CARTESIAN_POINT('Origin',(0.,0.,0.));
#15397=CARTESIAN_POINT('Origin',(0.,0.,0.));
#15398=CARTESIAN_POINT('',(0.,-7.34788079488412E-17,0.6));
#15399=CARTESIAN_POINT('Origin',(0.,0.,0.));
#15400=CARTESIAN_POINT('',(0.,0.,0.));
#15401=CARTESIAN_POINT('',(0.,0.,0.));
#15402=CARTESIAN_POINT('Origin',(-0.3,-1.,8.9));
#15403=CARTESIAN_POINT('',(-0.3,1.,9.04606079858305));
#15404=CARTESIAN_POINT('',(-0.3,-1.,9.04606079858305));
#15405=CARTESIAN_POINT('',(-0.3,-19.,9.04606079858305));
#15406=CARTESIAN_POINT('',(-0.3,1.,9.35));
#15407=CARTESIAN_POINT('',(-0.3,1.,9.45));
#15408=CARTESIAN_POINT('',(-0.3,-1.,9.35));
#15409=CARTESIAN_POINT('',(-0.3,-1.,9.35));
#15410=CARTESIAN_POINT('',(-0.3,-1.,9.35));
#15411=CARTESIAN_POINT('Origin',(0.,-1.,9.125));
#15412=CARTESIAN_POINT('',(0.3,-1.,9.04606079858305));
#15413=CARTESIAN_POINT('Origin',(0.,-1.,10.));
#15414=CARTESIAN_POINT('',(0.3,-1.,9.35));
#15415=CARTESIAN_POINT('',(0.3,-1.,9.35));
#15416=CARTESIAN_POINT('',(0.3,-1.,8.9));
#15417=CARTESIAN_POINT('Origin',(0.3,-1.,9.35));
#15418=CARTESIAN_POINT('',(0.3,1.,9.04606079858305));
#15419=CARTESIAN_POINT('',(0.3,-19.,9.04606079858305));
#15420=CARTESIAN_POINT('',(0.3,1.,9.35));
#15421=CARTESIAN_POINT('',(0.3,-1.,9.35));
#15422=CARTESIAN_POINT('',(0.3,1.,9.675));
#15423=CARTESIAN_POINT('Origin',(-0.3,-1.,9.35));
#15424=CARTESIAN_POINT('',(-0.15,1.,9.35));
#15425=CARTESIAN_POINT('Origin',(0.,-19.,10.));
#15426=CARTESIAN_POINT('',(-1.,1.,10.));
#15427=CARTESIAN_POINT('Origin',(0.,1.,10.));
#15428=CARTESIAN_POINT('',(-1.,-19.,10.));
#15429=CARTESIAN_POINT('',(-1.,-19.,10.));
#15430=CARTESIAN_POINT('Origin',(0.,-19.,10.));
#15431=CARTESIAN_POINT('Origin',(0.,1.,10.));
#15432=CARTESIAN_POINT('Origin',(0.,1.,10.));
#15433=CARTESIAN_POINT('Origin',(0.,-19.,10.));
#15434=CARTESIAN_POINT('',(0.,0.,0.));
#15435=CARTESIAN_POINT('Origin',(0.,-17.05,10.99));
#15436=CARTESIAN_POINT('',(0.172988438920051,-17.1690588089979,10.99));
#15437=CARTESIAN_POINT('',(0.172988438920051,-16.9309411910021,10.99));
#15438=CARTESIAN_POINT('',(0.172988438920051,-17.45,10.99));
#15439=CARTESIAN_POINT('Origin',(0.,-17.05,10.99));
#15440=CARTESIAN_POINT('Origin',(0.,-17.05,10.99));
#15441=CARTESIAN_POINT('',(-0.172988438920051,-17.1690588089979,10.99));
#15442=CARTESIAN_POINT('Ctrl Pts',(-0.172988438920051,-17.1690588089979,
10.99));
#15443=CARTESIAN_POINT('Ctrl Pts',(-0.165594865311311,-17.1798014223953,
10.9912919219764));
#15444=CARTESIAN_POINT('Ctrl Pts',(-0.157297138725604,-17.1896877093727,
10.992653949439));
#15445=CARTESIAN_POINT('Ctrl Pts',(-0.129892073845076,-17.2170927742533,
10.9967480843909));
#15446=CARTESIAN_POINT('Ctrl Pts',(-0.106330167759284,-17.233242056333,
10.9996958932764));
#15447=CARTESIAN_POINT('Ctrl Pts',(-0.0546129046324093,-17.2546977939649,
11.0038502947236));
#15448=CARTESIAN_POINT('Ctrl Pts',(-0.0264512308298518,-17.26,11.005));
#15449=CARTESIAN_POINT('Ctrl Pts',(0.0264512308298517,-17.26,11.005));
#15450=CARTESIAN_POINT('Ctrl Pts',(0.0546129046324092,-17.2546977939649,
11.0038502947236));
#15451=CARTESIAN_POINT('Ctrl Pts',(0.106330167759284,-17.233242056333,10.9996958932764));
#15452=CARTESIAN_POINT('Ctrl Pts',(0.129892073845076,-17.2170927742533,
10.9967480843909));
#15453=CARTESIAN_POINT('Ctrl Pts',(0.157297138725603,-17.1896877093727,
10.992653949439));
#15454=CARTESIAN_POINT('Ctrl Pts',(0.16559486531131,-17.1798014223953,10.9912919219764));
#15455=CARTESIAN_POINT('Ctrl Pts',(0.17298843892005,-17.1690588089979,10.99));
#15456=CARTESIAN_POINT('',(-0.21,-17.05,10.99));
#15457=CARTESIAN_POINT('Origin',(0.,-17.05,10.99));
#15458=CARTESIAN_POINT('',(-0.21,-17.05,11.4852272553384));
#15459=CARTESIAN_POINT('',(-0.21,-17.05,10.99));
#15460=CARTESIAN_POINT('',(0.21,-17.05,11.4852272553384));
#15461=CARTESIAN_POINT('Ctrl Pts',(0.21,-17.05,11.4852272553384));
#15462=CARTESIAN_POINT('Ctrl Pts',(0.21,-17.0764055269245,11.4852272553384));
#15463=CARTESIAN_POINT('Ctrl Pts',(0.204715737269596,-17.1045470740907,
11.4860041595441));
#15464=CARTESIAN_POINT('Ctrl Pts',(0.183273763036332,-17.1562762689051,
11.4888007328232));
#15465=CARTESIAN_POINT('Ctrl Pts',(0.167117923970393,-17.179866924128,11.4907789715758));
#15466=CARTESIAN_POINT('Ctrl Pts',(0.129867169887369,-17.217117678211,11.4944848114133));
#15467=CARTESIAN_POINT('Ctrl Pts',(0.106276408305765,-17.2332737100014,
11.4964545565713));
#15468=CARTESIAN_POINT('Ctrl Pts',(0.0545468514058993,-17.2547158248262,
11.4992316551565));
#15469=CARTESIAN_POINT('Ctrl Pts',(0.0264051785092816,-17.26,11.5));
#15470=CARTESIAN_POINT('Ctrl Pts',(-0.0264051785092815,-17.26,11.5));
#15471=CARTESIAN_POINT('Ctrl Pts',(-0.054546851405899,-17.2547158248262,
11.4992316551565));
#15472=CARTESIAN_POINT('Ctrl Pts',(-0.106276408305765,-17.2332737100014,
11.4964545565713));
#15473=CARTESIAN_POINT('Ctrl Pts',(-0.129867169887368,-17.217117678211,
11.4944848114133));
#15474=CARTESIAN_POINT('Ctrl Pts',(-0.167117923970393,-17.179866924128,
11.4907789715758));
#15475=CARTESIAN_POINT('Ctrl Pts',(-0.183273763036332,-17.1562762689051,
11.4888007328232));
#15476=CARTESIAN_POINT('Ctrl Pts',(-0.204715737269596,-17.1045470740907,
11.4860041595441));
#15477=CARTESIAN_POINT('Ctrl Pts',(-0.21,-17.0764055269245,11.4852272553384));
#15478=CARTESIAN_POINT('Ctrl Pts',(-0.21,-17.05,11.4852272553384));
#15479=CARTESIAN_POINT('Ctrl Pts',(-0.21,-17.05,11.4852272553384));
#15480=CARTESIAN_POINT('Ctrl Pts',(-0.21,-17.0235944730756,11.4852272553384));
#15481=CARTESIAN_POINT('Ctrl Pts',(-0.204715737269596,-16.9954529259093,
11.4860041595441));
#15482=CARTESIAN_POINT('Ctrl Pts',(-0.183273763036332,-16.9437237310949,
11.4888007328232));
#15483=CARTESIAN_POINT('Ctrl Pts',(-0.167117923970393,-16.920133075872,
11.4907789715758));
#15484=CARTESIAN_POINT('Ctrl Pts',(-0.129867169887369,-16.882882321789,
11.4944848114133));
#15485=CARTESIAN_POINT('Ctrl Pts',(-0.106276408305765,-16.8667262899986,
11.4964545565713));
#15486=CARTESIAN_POINT('Ctrl Pts',(-0.0545468514058993,-16.8452841751738,
11.4992316551565));
#15487=CARTESIAN_POINT('Ctrl Pts',(-0.0264051785092816,-16.84,11.5));
#15488=CARTESIAN_POINT('Ctrl Pts',(0.0264051785092815,-16.84,11.5));
#15489=CARTESIAN_POINT('Ctrl Pts',(0.0545468514058992,-16.8452841751738,
11.4992316551565));
#15490=CARTESIAN_POINT('Ctrl Pts',(0.106276408305765,-16.8667262899986,
11.4964545565713));
#15491=CARTESIAN_POINT('Ctrl Pts',(0.129867169887368,-16.882882321789,11.4944848114133));
#15492=CARTESIAN_POINT('Ctrl Pts',(0.167117923970393,-16.920133075872,11.4907789715758));
#15493=CARTESIAN_POINT('Ctrl Pts',(0.183273763036332,-16.9437237310949,
11.4888007328232));
#15494=CARTESIAN_POINT('Ctrl Pts',(0.204715737269596,-16.9954529259093,
11.4860041595441));
#15495=CARTESIAN_POINT('Ctrl Pts',(0.21,-17.0235944730756,11.4852272553384));
#15496=CARTESIAN_POINT('Ctrl Pts',(0.21,-17.05,11.4852272553384));
#15497=CARTESIAN_POINT('',(-0.172988438920051,-16.9309411910021,10.99));
#15498=CARTESIAN_POINT('Origin',(0.,-17.05,10.99));
#15499=CARTESIAN_POINT('Ctrl Pts',(0.17298843892005,-16.9309411910021,10.99));
#15500=CARTESIAN_POINT('Ctrl Pts',(0.16559486531131,-16.9201985776047,10.9912919219764));
#15501=CARTESIAN_POINT('Ctrl Pts',(0.157297138725604,-16.9103122906273,
10.9926539494391));
#15502=CARTESIAN_POINT('Ctrl Pts',(0.129892073845076,-16.8829072257467,
10.9967480843909));
#15503=CARTESIAN_POINT('Ctrl Pts',(0.106330167759284,-16.8667579436671,
10.9996958932764));
#15504=CARTESIAN_POINT('Ctrl Pts',(0.0546129046324093,-16.8453022060351,
11.0038502947236));
#15505=CARTESIAN_POINT('Ctrl Pts',(0.0264512308298517,-16.84,11.005));
#15506=CARTESIAN_POINT('Ctrl Pts',(-0.0264512308298517,-16.84,11.005));
#15507=CARTESIAN_POINT('Ctrl Pts',(-0.054612904632409,-16.8453022060351,
11.0038502947236));
#15508=CARTESIAN_POINT('Ctrl Pts',(-0.106330167759284,-16.8667579436671,
10.9996958932764));
#15509=CARTESIAN_POINT('Ctrl Pts',(-0.129892073845076,-16.8829072257467,
10.9967480843909));
#15510=CARTESIAN_POINT('Ctrl Pts',(-0.157297138725604,-16.9103122906273,
10.992653949439));
#15511=CARTESIAN_POINT('Ctrl Pts',(-0.165594865311311,-16.9201985776047,
10.9912919219764));
#15512=CARTESIAN_POINT('Ctrl Pts',(-0.172988438920051,-16.9309411910021,
10.99));
#15513=CARTESIAN_POINT('Origin',(0.,-17.05,10.99));
#15514=CARTESIAN_POINT('',(-0.172988438920051,-17.45,10.99));
#15515=CARTESIAN_POINT('Origin',(0.,-17.45,10.));
#15516=CARTESIAN_POINT('',(-1.005,-16.65,10.));
#15517=CARTESIAN_POINT('Origin',(0.,-16.65,10.));
#15518=CARTESIAN_POINT('',(-1.005,-17.45,10.));
#15519=CARTESIAN_POINT('',(-1.005,-17.45,10.));
#15520=CARTESIAN_POINT('Origin',(0.,-17.45,10.));
#15521=CARTESIAN_POINT('Origin',(0.,-17.45,10.));
#15522=CARTESIAN_POINT('',(-1.5,-16.65,10.));
#15523=CARTESIAN_POINT('Origin',(0.,-16.65,10.));
#15524=CARTESIAN_POINT('',(-1.5,-17.45,10.));
#15525=CARTESIAN_POINT('',(-1.5,-17.45,10.));
#15526=CARTESIAN_POINT('Origin',(0.,-17.45,10.));
#15527=CARTESIAN_POINT('Origin',(0.,-16.65,10.));
#15528=CARTESIAN_POINT('Origin',(0.,-17.45,10.));
#15529=CARTESIAN_POINT('',(0.,0.,0.));
#15530=CARTESIAN_POINT('Origin',(0.,-4.15,10.99));
#15531=CARTESIAN_POINT('',(0.172988438920051,-4.26905880899792,10.99));
#15532=CARTESIAN_POINT('',(0.172988438920051,-4.03094119100208,10.99));
#15533=CARTESIAN_POINT('',(0.172988438920051,-4.55,10.99));
#15534=CARTESIAN_POINT('Origin',(0.,-4.15,10.99));
#15535=CARTESIAN_POINT('Origin',(0.,-4.15,10.99));
#15536=CARTESIAN_POINT('',(-0.172988438920051,-4.26905880899792,10.99));
#15537=CARTESIAN_POINT('Ctrl Pts',(-0.172988438920051,-4.26905880899792,
10.99));
#15538=CARTESIAN_POINT('Ctrl Pts',(-0.165594865311311,-4.2798014223953,
10.9912919219764));
#15539=CARTESIAN_POINT('Ctrl Pts',(-0.157297138725605,-4.28968770937275,
10.992653949439));
#15540=CARTESIAN_POINT('Ctrl Pts',(-0.129892073845076,-4.31709277425327,
10.9967480843909));
#15541=CARTESIAN_POINT('Ctrl Pts',(-0.106330167759284,-4.33324205633295,
10.9996958932764));
#15542=CARTESIAN_POINT('Ctrl Pts',(-0.05461290463241,-4.35469779396491,
11.0038502947236));
#15543=CARTESIAN_POINT('Ctrl Pts',(-0.0264512308298516,-4.36,11.005));
#15544=CARTESIAN_POINT('Ctrl Pts',(0.0264512308298515,-4.36,11.005));
#15545=CARTESIAN_POINT('Ctrl Pts',(0.0546129046324099,-4.35469779396491,
11.0038502947236));
#15546=CARTESIAN_POINT('Ctrl Pts',(0.106330167759284,-4.33324205633295,
10.9996958932764));
#15547=CARTESIAN_POINT('Ctrl Pts',(0.129892073845076,-4.31709277425327,
10.9967480843909));
#15548=CARTESIAN_POINT('Ctrl Pts',(0.157297138725605,-4.28968770937275,
10.992653949439));
#15549=CARTESIAN_POINT('Ctrl Pts',(0.165594865311311,-4.2798014223953,10.9912919219764));
#15550=CARTESIAN_POINT('Ctrl Pts',(0.172988438920051,-4.26905880899792,
10.99));
#15551=CARTESIAN_POINT('',(-0.21,-4.15,10.99));
#15552=CARTESIAN_POINT('Origin',(0.,-4.15,10.99));
#15553=CARTESIAN_POINT('',(-0.21,-4.15,11.4852272553384));
#15554=CARTESIAN_POINT('',(-0.21,-4.15,10.99));
#15555=CARTESIAN_POINT('',(0.21,-4.15,11.4852272553384));
#15556=CARTESIAN_POINT('Ctrl Pts',(0.21,-4.15,11.4852272553384));
#15557=CARTESIAN_POINT('Ctrl Pts',(0.21,-4.17640552692446,11.4852272553384));
#15558=CARTESIAN_POINT('Ctrl Pts',(0.204715737269596,-4.20454707409071,
11.4860041595441));
#15559=CARTESIAN_POINT('Ctrl Pts',(0.183273763036332,-4.25627626890513,
11.4888007328232));
#15560=CARTESIAN_POINT('Ctrl Pts',(0.167117923970394,-4.27986692412796,
11.4907789715758));
#15561=CARTESIAN_POINT('Ctrl Pts',(0.129867169887369,-4.31711767821098,
11.4944848114133));
#15562=CARTESIAN_POINT('Ctrl Pts',(0.106276408305765,-4.33327371000135,
11.4964545565713));
#15563=CARTESIAN_POINT('Ctrl Pts',(0.0545468514059003,-4.35471582482622,
11.4992316551565));
#15564=CARTESIAN_POINT('Ctrl Pts',(0.0264051785092814,-4.36,11.5));
#15565=CARTESIAN_POINT('Ctrl Pts',(-0.0264051785092814,-4.36,11.5));
#15566=CARTESIAN_POINT('Ctrl Pts',(-0.0545468514059002,-4.35471582482622,
11.4992316551565));
#15567=CARTESIAN_POINT('Ctrl Pts',(-0.106276408305765,-4.33327371000135,
11.4964545565713));
#15568=CARTESIAN_POINT('Ctrl Pts',(-0.129867169887369,-4.31711767821098,
11.4944848114133));
#15569=CARTESIAN_POINT('Ctrl Pts',(-0.167117923970394,-4.27986692412796,
11.4907789715758));
#15570=CARTESIAN_POINT('Ctrl Pts',(-0.183273763036332,-4.25627626890513,
11.4888007328232));
#15571=CARTESIAN_POINT('Ctrl Pts',(-0.204715737269596,-4.20454707409071,
11.4860041595441));
#15572=CARTESIAN_POINT('Ctrl Pts',(-0.21,-4.17640552692446,11.4852272553384));
#15573=CARTESIAN_POINT('Ctrl Pts',(-0.21,-4.15,11.4852272553384));
#15574=CARTESIAN_POINT('Ctrl Pts',(-0.21,-4.15,11.4852272553384));
#15575=CARTESIAN_POINT('Ctrl Pts',(-0.21,-4.12359447307555,11.4852272553384));
#15576=CARTESIAN_POINT('Ctrl Pts',(-0.204715737269596,-4.09545292590929,
11.4860041595441));
#15577=CARTESIAN_POINT('Ctrl Pts',(-0.183273763036332,-4.04372373109487,
11.4888007328232));
#15578=CARTESIAN_POINT('Ctrl Pts',(-0.167117923970394,-4.02013307587204,
11.4907789715758));
#15579=CARTESIAN_POINT('Ctrl Pts',(-0.129867169887369,-3.98288232178902,
11.4944848114133));
#15580=CARTESIAN_POINT('Ctrl Pts',(-0.106276408305765,-3.96672628999865,
11.4964545565713));
#15581=CARTESIAN_POINT('Ctrl Pts',(-0.0545468514059,-3.94528417517378,11.4992316551565));
#15582=CARTESIAN_POINT('Ctrl Pts',(-0.0264051785092814,-3.94,11.5));
#15583=CARTESIAN_POINT('Ctrl Pts',(0.0264051785092813,-3.94,11.5));
#15584=CARTESIAN_POINT('Ctrl Pts',(0.0545468514058999,-3.94528417517378,
11.4992316551565));
#15585=CARTESIAN_POINT('Ctrl Pts',(0.106276408305765,-3.96672628999865,
11.4964545565713));
#15586=CARTESIAN_POINT('Ctrl Pts',(0.129867169887369,-3.98288232178902,
11.4944848114133));
#15587=CARTESIAN_POINT('Ctrl Pts',(0.167117923970394,-4.02013307587204,
11.4907789715758));
#15588=CARTESIAN_POINT('Ctrl Pts',(0.183273763036331,-4.04372373109487,
11.4888007328232));
#15589=CARTESIAN_POINT('Ctrl Pts',(0.204715737269596,-4.09545292590929,
11.4860041595441));
#15590=CARTESIAN_POINT('Ctrl Pts',(0.21,-4.12359447307555,11.4852272553384));
#15591=CARTESIAN_POINT('Ctrl Pts',(0.21,-4.15,11.4852272553384));
#15592=CARTESIAN_POINT('',(-0.172988438920051,-4.03094119100208,10.99));
#15593=CARTESIAN_POINT('Origin',(0.,-4.15,10.99));
#15594=CARTESIAN_POINT('Ctrl Pts',(0.172988438920051,-4.03094119100208,
10.99));
#15595=CARTESIAN_POINT('Ctrl Pts',(0.16559486531131,-4.0201985776047,10.9912919219764));
#15596=CARTESIAN_POINT('Ctrl Pts',(0.157297138725604,-4.01031229062725,
10.992653949439));
#15597=CARTESIAN_POINT('Ctrl Pts',(0.129892073845076,-3.98290722574673,
10.9967480843909));
#15598=CARTESIAN_POINT('Ctrl Pts',(0.106330167759284,-3.96675794366705,
10.9996958932764));
#15599=CARTESIAN_POINT('Ctrl Pts',(0.0546129046324106,-3.94530220603509,
11.0038502947236));
#15600=CARTESIAN_POINT('Ctrl Pts',(0.0264512308298516,-3.94,11.005));
#15601=CARTESIAN_POINT('Ctrl Pts',(-0.0264512308298516,-3.94,11.005));
#15602=CARTESIAN_POINT('Ctrl Pts',(-0.0546129046324106,-3.94530220603509,
11.0038502947236));
#15603=CARTESIAN_POINT('Ctrl Pts',(-0.106330167759284,-3.96675794366705,
10.9996958932764));
#15604=CARTESIAN_POINT('Ctrl Pts',(-0.129892073845076,-3.98290722574673,
10.9967480843909));
#15605=CARTESIAN_POINT('Ctrl Pts',(-0.157297138725604,-4.01031229062725,
10.992653949439));
#15606=CARTESIAN_POINT('Ctrl Pts',(-0.16559486531131,-4.0201985776047,10.9912919219764));
#15607=CARTESIAN_POINT('Ctrl Pts',(-0.172988438920051,-4.03094119100208,
10.99));
#15608=CARTESIAN_POINT('Origin',(0.,-4.15,10.99));
#15609=CARTESIAN_POINT('',(-0.172988438920051,-4.55,10.99));
#15610=CARTESIAN_POINT('Origin',(0.,-4.55,10.));
#15611=CARTESIAN_POINT('',(-1.005,-3.75,10.));
#15612=CARTESIAN_POINT('Origin',(0.,-3.75,10.));
#15613=CARTESIAN_POINT('',(-1.005,-4.55,10.));
#15614=CARTESIAN_POINT('',(-1.005,-4.55,10.));
#15615=CARTESIAN_POINT('Origin',(0.,-4.55,10.));
#15616=CARTESIAN_POINT('Origin',(0.,-4.55,10.));
#15617=CARTESIAN_POINT('',(-1.5,-3.75,10.));
#15618=CARTESIAN_POINT('Origin',(0.,-3.75,10.));
#15619=CARTESIAN_POINT('',(-1.5,-4.55,10.));
#15620=CARTESIAN_POINT('',(-1.5,-4.55,10.));
#15621=CARTESIAN_POINT('Origin',(0.,-4.55,10.));
#15622=CARTESIAN_POINT('Origin',(0.,-3.75,10.));
#15623=CARTESIAN_POINT('Origin',(0.,-4.55,10.));
#15624=CARTESIAN_POINT('',(0.,0.,0.));
#15625=CARTESIAN_POINT('Origin',(0.,-16.65,10.));
#15626=CARTESIAN_POINT('',(-1.005,-15.85,10.));
#15627=CARTESIAN_POINT('Origin',(0.,-15.85,10.));
#15628=CARTESIAN_POINT('',(-1.005,-16.65,10.));
#15629=CARTESIAN_POINT('',(-1.005,-16.65,10.));
#15630=CARTESIAN_POINT('Origin',(0.,-16.65,10.));
#15631=CARTESIAN_POINT('Origin',(0.,-16.65,10.));
#15632=CARTESIAN_POINT('',(-1.3,-15.85,10.));
#15633=CARTESIAN_POINT('Origin',(0.,-15.85,10.));
#15634=CARTESIAN_POINT('',(-1.3,-16.65,10.));
#15635=CARTESIAN_POINT('',(-1.3,-16.65,10.));
#15636=CARTESIAN_POINT('Origin',(0.,-16.65,10.));
#15637=CARTESIAN_POINT('Origin',(0.,-15.85,10.));
#15638=CARTESIAN_POINT('Origin',(0.,-16.65,10.));
#15639=CARTESIAN_POINT('',(0.,0.,0.));
#15640=CARTESIAN_POINT('Origin',(2.,1.,10.));
#15641=CARTESIAN_POINT('',(1.5775,1.,10.2673831520496));
#15642=CARTESIAN_POINT('',(1.5775,1.5,10.2673831520496));
#15643=CARTESIAN_POINT('',(1.5775,1.,10.2673831520496));
#15644=CARTESIAN_POINT('',(1.5775,1.,9.73261684795036));
#15645=CARTESIAN_POINT('Origin',(2.,1.,10.));
#15646=CARTESIAN_POINT('',(1.5775,1.5,9.73261684795036));
#15647=CARTESIAN_POINT('',(1.5775,1.,9.73261684795036));
#15648=CARTESIAN_POINT('Origin',(2.,1.5,10.));
#15649=CARTESIAN_POINT('Origin',(0.,1.5,10.));
#15650=CARTESIAN_POINT('Origin',(0.,1.5,10.));
#15651=CARTESIAN_POINT('',(-0.3,1.5,9.04606079858305));
#15652=CARTESIAN_POINT('',(-0.3,1.5,8.72));
#15653=CARTESIAN_POINT('',(-0.3,1.5,9.36));
#15654=CARTESIAN_POINT('',(0.3,1.5,8.72));
#15655=CARTESIAN_POINT('',(0.15,1.5,8.72));
#15656=CARTESIAN_POINT('',(0.3,1.5,9.04606079858305));
#15657=CARTESIAN_POINT('',(0.3,1.5,10.));
#15658=CARTESIAN_POINT('Origin',(0.,1.5,10.));
#15659=CARTESIAN_POINT('Origin',(2.,-0.1,10.));
#15660=CARTESIAN_POINT('',(1.66,-0.1,10.));
#15661=CARTESIAN_POINT('Origin',(2.,-0.1,10.));
#15662=CARTESIAN_POINT('',(1.66,1.,10.));
#15663=CARTESIAN_POINT('',(1.66,-0.1,10.));
#15664=CARTESIAN_POINT('Origin',(2.,1.,10.));
#15665=CARTESIAN_POINT('Origin',(2.,-0.1,10.));
#15666=CARTESIAN_POINT('Origin',(0.,-1.3,10.99));
#15667=CARTESIAN_POINT('',(-0.141067359796645,-1.14443650813895,10.99));
#15668=CARTESIAN_POINT('',(-0.141067359796645,-1.45556349186105,10.99));
#15669=CARTESIAN_POINT('',(-0.141067359796645,-1.5,10.99));
#15670=CARTESIAN_POINT('Origin',(0.,-1.3,10.99));
#15671=CARTESIAN_POINT('Origin',(0.,-1.3,10.99));
#15672=CARTESIAN_POINT('',(0.141067359796645,-1.14443650813895,10.99));
#15673=CARTESIAN_POINT('Ctrl Pts',(0.141067359796645,-1.14443650813895,
10.99));
#15674=CARTESIAN_POINT('Ctrl Pts',(0.123818356698215,-1.1287948476368,10.9924578498245));
#15675=CARTESIAN_POINT('Ctrl Pts',(0.102998643109694,-1.11537595666898,
10.9949381930495));
#15676=CARTESIAN_POINT('Ctrl Pts',(0.054614114398353,-1.09530253627557,
10.9988444923724));
#15677=CARTESIAN_POINT('Ctrl Pts',(0.0264520736824499,-1.09,11.));
#15678=CARTESIAN_POINT('Ctrl Pts',(-0.0264520736824498,-1.09,11.));
#15679=CARTESIAN_POINT('Ctrl Pts',(-0.0546141143983528,-1.09530253627557,
10.9988444923724));
#15680=CARTESIAN_POINT('Ctrl Pts',(-0.102998643109694,-1.11537595666898,
10.9949381930495));
#15681=CARTESIAN_POINT('Ctrl Pts',(-0.123818356698214,-1.1287948476368,
10.9924578498245));
#15682=CARTESIAN_POINT('Ctrl Pts',(-0.141067359796645,-1.14443650813895,
10.99));
#15683=CARTESIAN_POINT('',(0.141067359796645,-1.45556349186105,10.99));
#15684=CARTESIAN_POINT('Origin',(0.,-1.3,10.99));
#15685=CARTESIAN_POINT('',(0.0640312423743287,-1.5,10.9979478944314));
#15686=CARTESIAN_POINT('Ctrl Pts',(0.0640312423743287,-1.5,10.9979478944314));
#15687=CARTESIAN_POINT('Ctrl Pts',(0.0695863834759532,-1.49822148706849,
10.9975914604048));
#15688=CARTESIAN_POINT('Ctrl Pts',(0.0750776578932034,-1.49620769804413,
10.9971923790166));
#15689=CARTESIAN_POINT('Ctrl Pts',(0.102998643109694,-1.48462404333102,
10.9949381930495));
#15690=CARTESIAN_POINT('Ctrl Pts',(0.123818356698214,-1.4712051523632,10.9924578498245));
#15691=CARTESIAN_POINT('Ctrl Pts',(0.141067359796645,-1.45556349186105,
10.99));
#15692=CARTESIAN_POINT('',(0.0640312423743287,-1.5,11.5987182365883));
#15693=CARTESIAN_POINT('',(0.0640312423743287,-1.5,10.99));
#15694=CARTESIAN_POINT('',(-0.0640312423743287,-1.5,11.5987182365883));
#15695=CARTESIAN_POINT('Ctrl Pts',(-0.0640312423743287,-1.5,11.5987182365883));
#15696=CARTESIAN_POINT('Ctrl Pts',(-0.0695623721690265,-1.49822917443756,
11.5984967059243));
#15697=CARTESIAN_POINT('Ctrl Pts',(-0.0750312749053373,-1.49622475645458,
11.5982488123351));
#15698=CARTESIAN_POINT('Ctrl Pts',(-0.106271159541076,-1.48327680083123,
11.5966769093301));
#15699=CARTESIAN_POINT('Ctrl Pts',(-0.129864750292352,-1.467120097806,11.5948307595328));
#15700=CARTESIAN_POINT('Ctrl Pts',(-0.167120287247804,-1.42986456085055,
11.5913581688701));
#15701=CARTESIAN_POINT('Ctrl Pts',(-0.183276841782292,-1.4062710523005,
11.5895050296478));
#15702=CARTESIAN_POINT('Ctrl Pts',(-0.20471752266132,-1.35454055536511,
11.586886062954));
#15703=CARTESIAN_POINT('Ctrl Pts',(-0.21,-1.32640093420375,11.5861588823318));
#15704=CARTESIAN_POINT('Ctrl Pts',(-0.21,-1.27359906579625,11.5861588823318));
#15705=CARTESIAN_POINT('Ctrl Pts',(-0.20471752266132,-1.24545944463489,
11.586886062954));
#15706=CARTESIAN_POINT('Ctrl Pts',(-0.183276841782292,-1.1937289476995,
11.5895050296478));
#15707=CARTESIAN_POINT('Ctrl Pts',(-0.167120287247804,-1.17013543914945,
11.5913581688701));
#15708=CARTESIAN_POINT('Ctrl Pts',(-0.129864750292352,-1.132879902194,11.5948307595328));
#15709=CARTESIAN_POINT('Ctrl Pts',(-0.106271159541076,-1.11672319916877,
11.5966769093301));
#15710=CARTESIAN_POINT('Ctrl Pts',(-0.0545403836274686,-1.0952824096556,
11.5992798562698));
#15711=CARTESIAN_POINT('Ctrl Pts',(-0.0264006657112965,-1.09,11.6));
#15712=CARTESIAN_POINT('Ctrl Pts',(0.0264006657112964,-1.09,11.6));
#15713=CARTESIAN_POINT('Ctrl Pts',(0.0545403836274687,-1.0952824096556,
11.5992798562698));
#15714=CARTESIAN_POINT('Ctrl Pts',(0.106271159541076,-1.11672319916877,
11.5966769093301));
#15715=CARTESIAN_POINT('Ctrl Pts',(0.129864750292352,-1.132879902194,11.5948307595328));
#15716=CARTESIAN_POINT('Ctrl Pts',(0.167120287247804,-1.17013543914945,
11.5913581688701));
#15717=CARTESIAN_POINT('Ctrl Pts',(0.183276841782292,-1.1937289476995,11.5895050296478));
#15718=CARTESIAN_POINT('Ctrl Pts',(0.20471752266132,-1.24545944463489,11.586886062954));
#15719=CARTESIAN_POINT('Ctrl Pts',(0.21,-1.27359906579625,11.5861588823318));
#15720=CARTESIAN_POINT('Ctrl Pts',(0.21,-1.3,11.5861588823318));
#15721=CARTESIAN_POINT('Ctrl Pts',(0.21,-1.32640093420375,11.5861588823318));
#15722=CARTESIAN_POINT('Ctrl Pts',(0.20471752266132,-1.35454055536511,11.586886062954));
#15723=CARTESIAN_POINT('Ctrl Pts',(0.183276841782292,-1.4062710523005,11.5895050296478));
#15724=CARTESIAN_POINT('Ctrl Pts',(0.167120287247804,-1.42986456085055,
11.5913581688701));
#15725=CARTESIAN_POINT('Ctrl Pts',(0.129864750292352,-1.467120097806,11.5948307595328));
#15726=CARTESIAN_POINT('Ctrl Pts',(0.106271159541076,-1.48327680083123,
11.5966769093301));
#15727=CARTESIAN_POINT('Ctrl Pts',(0.0750312749053373,-1.49622475645458,
11.5982488123351));
#15728=CARTESIAN_POINT('Ctrl Pts',(0.0695623721690265,-1.49822917443756,
11.5984967059243));
#15729=CARTESIAN_POINT('Ctrl Pts',(0.0640312423743287,-1.5,11.5987182365883));
#15730=CARTESIAN_POINT('',(-0.0640312423743287,-1.5,10.9979478944314));
#15731=CARTESIAN_POINT('',(-0.0640312423743287,-1.5,10.99));
#15732=CARTESIAN_POINT('Ctrl Pts',(-0.141067359796645,-1.45556349186105,
10.99));
#15733=CARTESIAN_POINT('Ctrl Pts',(-0.123818356698214,-1.4712051523632,
10.9924578498245));
#15734=CARTESIAN_POINT('Ctrl Pts',(-0.102998643109694,-1.48462404333102,
10.9949381930495));
#15735=CARTESIAN_POINT('Ctrl Pts',(-0.0750776578932034,-1.49620769804413,
10.9971923790166));
#15736=CARTESIAN_POINT('Ctrl Pts',(-0.0695863834759533,-1.49822148706849,
10.9975914604048));
#15737=CARTESIAN_POINT('Ctrl Pts',(-0.0640312423743287,-1.5,10.9979478944314));
#15738=CARTESIAN_POINT('Origin',(0.,-1.3,10.99));
#15739=CARTESIAN_POINT('',(0.141067359796645,-1.5,10.99));
#15740=CARTESIAN_POINT('Origin',(0.,-1.5,10.));
#15741=CARTESIAN_POINT('',(-0.3,-1.5,9.04606079858305));
#15742=CARTESIAN_POINT('Origin',(0.,-1.5,10.));
#15743=CARTESIAN_POINT('',(-0.3,-1.5,9.04606079858305));
#15744=CARTESIAN_POINT('',(0.3,-1.5,9.04606079858305));
#15745=CARTESIAN_POINT('',(0.3,-1.5,9.04606079858305));
#15746=CARTESIAN_POINT('Origin',(0.,-1.5,10.));
#15747=CARTESIAN_POINT('Origin',(-0.3,-1.6,8.72));
#15748=CARTESIAN_POINT('',(-0.3,-1.5,8.72));
#15749=CARTESIAN_POINT('',(-0.3,-1.5,9.36));
#15750=CARTESIAN_POINT('',(-0.3,-1.6,8.72));
#15751=CARTESIAN_POINT('Origin',(0.3,-1.6,8.72));
#15752=CARTESIAN_POINT('',(0.3,-1.5,8.72));
#15753=CARTESIAN_POINT('',(0.15,-1.5,8.72));
#15754=CARTESIAN_POINT('',(0.3,-1.6,8.72));
#15755=CARTESIAN_POINT('Origin',(0.3,-1.6,10.));
#15756=CARTESIAN_POINT('',(0.3,-1.5,10.));
#15757=CARTESIAN_POINT('Origin',(0.,1.,10.));
#15758=CARTESIAN_POINT('',(-4.,1.,10.));
#15759=CARTESIAN_POINT('Origin',(0.,1.,10.));
#15760=CARTESIAN_POINT('Origin',(0.,1.,10.));
#15761=CARTESIAN_POINT('Origin',(0.,-1.,10.));
#15762=CARTESIAN_POINT('',(-4.,-1.,10.));
#15763=CARTESIAN_POINT('Origin',(0.,-1.,10.));
#15764=CARTESIAN_POINT('',(-1.6,-1.,10.));
#15765=CARTESIAN_POINT('Origin',(0.,-1.,10.));
#15766=CARTESIAN_POINT('Origin',(0.,-1.,10.));
#15767=CARTESIAN_POINT('',(-4.,-1.,10.));
#15768=CARTESIAN_POINT('Origin',(0.,-1.5,10.));
#15769=CARTESIAN_POINT('',(-1.6,-1.5,10.));
#15770=CARTESIAN_POINT('',(-1.6,-1.5,10.));
#15771=CARTESIAN_POINT('Origin',(0.,-1.5,10.));
#15772=CARTESIAN_POINT('Origin',(0.,-1.5,10.));
#15773=CARTESIAN_POINT('Origin',(0.,-1.5,10.));
#15774=CARTESIAN_POINT('Origin',(0.,-1.5,10.));
#15775=CARTESIAN_POINT('',(0.,0.,0.));
#15776=CARTESIAN_POINT('Origin',(2.,2.7,10.));
#15777=CARTESIAN_POINT('',(1.835,2.7,10.));
#15778=CARTESIAN_POINT('Origin',(2.,2.7,10.));
#15779=CARTESIAN_POINT('',(1.835,3.8,10.));
#15780=CARTESIAN_POINT('',(1.835,2.7,10.));
#15781=CARTESIAN_POINT('Origin',(2.,3.8,10.));
#15782=CARTESIAN_POINT('Origin',(2.,2.7,10.));
#15783=CARTESIAN_POINT('Origin',(2.,1.,10.));
#15784=CARTESIAN_POINT('',(1.5,1.,10.));
#15785=CARTESIAN_POINT('Origin',(2.,1.,10.));
#15786=CARTESIAN_POINT('',(1.6,1.,10.));
#15787=CARTESIAN_POINT('Origin',(2.,1.,10.));
#15788=CARTESIAN_POINT('Origin',(2.,1.,10.));
#15789=CARTESIAN_POINT('',(1.5,3.8,10.));
#15790=CARTESIAN_POINT('Origin',(2.,3.8,10.));
#15791=CARTESIAN_POINT('',(1.5,1.,10.));
#15792=CARTESIAN_POINT('Origin',(2.,3.8,10.));
#15793=CARTESIAN_POINT('Origin',(2.,0.,10.));
#15794=CARTESIAN_POINT('',(1.6,0.,10.));
#15795=CARTESIAN_POINT('',(1.6,0.,10.));
#15796=CARTESIAN_POINT('Origin',(2.,0.,10.));
#15797=CARTESIAN_POINT('Origin',(2.,0.,10.));
#15798=CARTESIAN_POINT('',(0.,0.,0.));
#15799=CARTESIAN_POINT('Origin',(2.,1.5,10.));
#15800=CARTESIAN_POINT('',(1.495,2.5,10.));
#15801=CARTESIAN_POINT('Origin',(2.,2.5,10.));
#15802=CARTESIAN_POINT('',(1.495,1.5,10.));
#15803=CARTESIAN_POINT('',(1.495,1.5,10.));
#15804=CARTESIAN_POINT('Origin',(2.,1.5,10.));
#15805=CARTESIAN_POINT('Origin',(2.,1.5,10.));
#15806=CARTESIAN_POINT('',(1.3,2.5,10.));
#15807=CARTESIAN_POINT('Origin',(2.,2.5,10.));
#15808=CARTESIAN_POINT('',(1.3,1.5,10.));
#15809=CARTESIAN_POINT('',(1.3,1.5,10.));
#15810=CARTESIAN_POINT('Origin',(2.,1.5,10.));
#15811=CARTESIAN_POINT('Origin',(2.,2.5,10.));
#15812=CARTESIAN_POINT('Origin',(2.,1.5,10.));
#15813=CARTESIAN_POINT('',(0.,0.,0.));
#15814=CARTESIAN_POINT('Origin',(2.,3.4,10.));
#15815=CARTESIAN_POINT('',(1.495,3.8,10.));
#15816=CARTESIAN_POINT('Origin',(2.,3.8,10.));
#15817=CARTESIAN_POINT('',(1.495,3.4,10.));
#15818=CARTESIAN_POINT('',(1.495,3.4,10.));
#15819=CARTESIAN_POINT('Origin',(2.,3.4,10.));
#15820=CARTESIAN_POINT('Origin',(2.,3.4,10.));
#15821=CARTESIAN_POINT('',(1.3,3.8,10.));
#15822=CARTESIAN_POINT('Origin',(2.,3.8,10.));
#15823=CARTESIAN_POINT('',(1.3,3.4,10.));
#15824=CARTESIAN_POINT('',(1.3,3.4,10.));
#15825=CARTESIAN_POINT('Origin',(2.,3.4,10.));
#15826=CARTESIAN_POINT('Origin',(2.,3.8,10.));
#15827=CARTESIAN_POINT('Origin',(2.,3.4,10.));
#15828=CARTESIAN_POINT('',(0.,0.,0.));
#15829=CARTESIAN_POINT('Origin',(2.,3.8,10.));
#15830=CARTESIAN_POINT('',(1.775,4.,10.));
#15831=CARTESIAN_POINT('Origin',(2.,4.,10.));
#15832=CARTESIAN_POINT('',(1.775,3.8,10.));
#15833=CARTESIAN_POINT('',(1.775,3.8,10.));
#15834=CARTESIAN_POINT('Origin',(2.,3.8,10.));
#15835=CARTESIAN_POINT('Origin',(2.,3.8,10.));
#15836=CARTESIAN_POINT('',(1.2,4.,10.));
#15837=CARTESIAN_POINT('Origin',(2.,4.,10.));
#15838=CARTESIAN_POINT('',(1.2,3.8,10.));
#15839=CARTESIAN_POINT('',(1.2,3.8,10.));
#15840=CARTESIAN_POINT('Origin',(2.,3.8,10.));
#15841=CARTESIAN_POINT('Origin',(2.,4.,10.));
#15842=CARTESIAN_POINT('Origin',(2.,3.8,10.));
#15843=CARTESIAN_POINT('',(0.,0.,0.));
#15844=CARTESIAN_POINT('Origin',(-1.,0.,0.35));
#15845=CARTESIAN_POINT('',(-1.,-0.26,0.6));
#15846=CARTESIAN_POINT('',(-1.,-0.3,0.56));
#15847=CARTESIAN_POINT('',(-1.,-0.2675,0.5925));
#15848=CARTESIAN_POINT('',(-1.,0.26,0.6));
#15849=CARTESIAN_POINT('',(-1.,0.,0.6));
#15850=CARTESIAN_POINT('',(-1.,0.3,0.56));
#15851=CARTESIAN_POINT('',(-1.,0.2675,0.5925));
#15852=CARTESIAN_POINT('',(-1.,0.3,0.04));
#15853=CARTESIAN_POINT('',(-1.,0.3,0.175));
#15854=CARTESIAN_POINT('',(-1.,0.26,0.));
#15855=CARTESIAN_POINT('',(-1.,0.2925,0.0325));
#15856=CARTESIAN_POINT('',(-1.,-0.26,0.));
#15857=CARTESIAN_POINT('',(-1.,0.,0.));
#15858=CARTESIAN_POINT('',(-1.,-0.3,0.04));
#15859=CARTESIAN_POINT('',(-1.,-0.2925,0.0325));
#15860=CARTESIAN_POINT('',(-1.,-0.3,0.175));
#15861=CARTESIAN_POINT('Origin',(0.75,0.28,0.02));
#15862=CARTESIAN_POINT('',(1.,0.3,0.04));
#15863=CARTESIAN_POINT('',(0.75,0.3,0.04));
#15864=CARTESIAN_POINT('',(1.,0.26,0.));
#15865=CARTESIAN_POINT('',(1.,0.2925,0.0325));
#15866=CARTESIAN_POINT('',(0.75,0.26,0.));
#15867=CARTESIAN_POINT('Origin',(1.5,0.3,0.));
#15868=CARTESIAN_POINT('',(1.,0.3,0.56));
#15869=CARTESIAN_POINT('',(0.75,0.3,0.56));
#15870=CARTESIAN_POINT('',(1.,0.3,0.175));
#15871=CARTESIAN_POINT('Origin',(0.75,0.28,0.58));
#15872=CARTESIAN_POINT('',(1.,0.26,0.6));
#15873=CARTESIAN_POINT('',(0.75,0.26,0.6));
#15874=CARTESIAN_POINT('',(1.,0.2675,0.5925));
#15875=CARTESIAN_POINT('Origin',(0.,0.,0.6));
#15876=CARTESIAN_POINT('',(1.,-0.26,0.6));
#15877=CARTESIAN_POINT('',(-0.75,-0.26,0.6));
#15878=CARTESIAN_POINT('',(1.,0.,0.6));
#15879=CARTESIAN_POINT('Origin',(1.,0.,0.35));
#15880=CARTESIAN_POINT('',(1.,-0.26,0.));
#15881=CARTESIAN_POINT('',(1.,-0.3,0.04));
#15882=CARTESIAN_POINT('',(1.,-0.2925,0.0325));
#15883=CARTESIAN_POINT('',(1.,0.,0.));
#15884=CARTESIAN_POINT('',(1.,-0.3,0.56));
#15885=CARTESIAN_POINT('',(1.,-0.2675,0.5925));
#15886=CARTESIAN_POINT('',(1.,-0.3,0.175));
#15887=CARTESIAN_POINT('Origin',(0.,0.,0.));
#15888=CARTESIAN_POINT('',(-0.75,-0.26,0.));
#15889=CARTESIAN_POINT('Origin',(-0.75,-0.28,0.58));
#15890=CARTESIAN_POINT('',(-0.75,-0.3,0.56));
#15891=CARTESIAN_POINT('Origin',(-0.75,-0.28,0.02));
#15892=CARTESIAN_POINT('',(-0.75,-0.3,0.04));
#15893=CARTESIAN_POINT('Origin',(-1.5,-0.3,0.));
#15894=CARTESIAN_POINT('',(0.,0.,0.));
#15895=CARTESIAN_POINT('Origin',(0.0721687836487032,0.,-0.125));
#15896=CARTESIAN_POINT('',(0.0721687836487032,0.,-0.125));
#15897=CARTESIAN_POINT('',(0.144337567297406,0.,0.));
#15898=CARTESIAN_POINT('',(0.117710979560879,0.,-0.0461186027918559));
#15899=CARTESIAN_POINT('',(0.0721687836487032,-0.25,-0.125));
#15900=CARTESIAN_POINT('',(0.0721687836487032,0.,-0.125));
#15901=CARTESIAN_POINT('',(0.144337567297406,-0.25,0.));
#15902=CARTESIAN_POINT('',(0.144337567297406,-0.25,0.));
#15903=CARTESIAN_POINT('',(0.144337567297406,0.,0.));
#15904=CARTESIAN_POINT('Origin',(-0.0721687836487032,0.,-0.125));
#15905=CARTESIAN_POINT('',(-0.0721687836487032,0.,-0.125));
#15906=CARTESIAN_POINT('',(0.0739156081756484,0.,-0.125));
#15907=CARTESIAN_POINT('',(-0.0721687836487032,-0.25,-0.125));
#15908=CARTESIAN_POINT('',(-0.0721687836487032,0.,-0.125));
#15909=CARTESIAN_POINT('',(0.0721687836487032,-0.25,-0.125));
#15910=CARTESIAN_POINT('Origin',(-0.144337567297406,0.,-4.16333634234434E-17));
#15911=CARTESIAN_POINT('',(-0.144337567297406,0.,-1.76762539787485E-17));
#15912=CARTESIAN_POINT('',(-0.0987953713852306,0.,-0.0788813972081442));
#15913=CARTESIAN_POINT('',(-0.144337567297406,-0.25,-2.77555756156289E-17));
#15914=CARTESIAN_POINT('',(-0.144337567297406,0.,-1.76762539787485E-17));
#15915=CARTESIAN_POINT('',(-0.0721687836487032,-0.25,-0.125));
#15916=CARTESIAN_POINT('Origin',(-0.0721687836487033,0.,0.125));
#15917=CARTESIAN_POINT('',(-0.0721687836487033,0.,0.125));
#15918=CARTESIAN_POINT('',(-0.0627109795608791,0.,0.141381397208144));
#15919=CARTESIAN_POINT('',(-0.0721687836487033,-0.25,0.125));
#15920=CARTESIAN_POINT('',(-0.0721687836487033,0.,0.125));
#15921=CARTESIAN_POINT('',(-0.144337567297406,-0.25,-1.76762539787485E-17));
#15922=CARTESIAN_POINT('Origin',(0.0721687836487032,0.,0.125));
#15923=CARTESIAN_POINT('',(0.0721687836487032,0.,0.125));
#15924=CARTESIAN_POINT('',(0.146084391824352,0.,0.125));
#15925=CARTESIAN_POINT('',(0.0721687836487032,-0.25,0.125));
#15926=CARTESIAN_POINT('',(0.0721687836487032,0.,0.125));
#15927=CARTESIAN_POINT('',(-0.0721687836487033,-0.25,0.125));
#15928=CARTESIAN_POINT('Origin',(0.144337567297406,0.,0.));
#15929=CARTESIAN_POINT('',(0.153795371385231,0.,-0.0163813972081441));
#15930=CARTESIAN_POINT('',(0.0721687836487032,-0.25,0.125));
#15931=CARTESIAN_POINT('Origin',(0.,-0.25,0.));
#15932=CARTESIAN_POINT('Origin',(0.22,0.,0.));
#15933=CARTESIAN_POINT('',(-0.22,-8.67361737988404E-18,-2.69422295812418E-17));
#15934=CARTESIAN_POINT('Origin',(0.,0.,0.));
#15935=CARTESIAN_POINT('Origin',(0.,-0.015,0.));
#15936=CARTESIAN_POINT('',(-0.24505,-0.02505,-3.00099698131059E-17));
#15937=CARTESIAN_POINT('Origin',(0.,-0.02505,0.));
#15938=CARTESIAN_POINT('',(-0.235,-0.015,-2.87791997799628E-17));
#15939=CARTESIAN_POINT('Origin',(0.,-0.3775,0.));
#15940=CARTESIAN_POINT('',(-0.24505,-0.72995,3.00099698131059E-17));
#15941=CARTESIAN_POINT('Origin',(0.,-0.72995,0.));
#15942=CARTESIAN_POINT('',(-0.24505,-0.3775,-3.00099698131059E-17));
#15943=CARTESIAN_POINT('Origin',(0.,-0.7625,0.));
#15944=CARTESIAN_POINT('',(-0.175,-0.8,-2.14313189850787E-17));
#15945=CARTESIAN_POINT('Origin',(0.,-0.8,0.));
#15946=CARTESIAN_POINT('',(-0.2125,-0.7625,-2.60237444818813E-17));
#15947=CARTESIAN_POINT('Origin',(0.,-0.8,0.));
#15948=CARTESIAN_POINT('',(0.,0.,0.));
#15949=CARTESIAN_POINT('',(0.,0.,0.));
#15950=CARTESIAN_POINT('Origin',(2.,2.4,10.));
#15951=CARTESIAN_POINT('',(0.5,2.5,10.));
#15952=CARTESIAN_POINT('Origin',(2.,2.5,10.));
#15953=CARTESIAN_POINT('',(0.5,3.4,10.));
#15954=CARTESIAN_POINT('',(0.5,2.4,10.));
#15955=CARTESIAN_POINT('Origin',(2.,3.4,10.));
#15956=CARTESIAN_POINT('Origin',(12.,2.4,10.));
#15957=CARTESIAN_POINT('',(10.5,2.5,10.));
#15958=CARTESIAN_POINT('Origin',(12.,2.5,10.));
#15959=CARTESIAN_POINT('',(10.5,3.4,10.));
#15960=CARTESIAN_POINT('',(10.5,2.4,10.));
#15961=CARTESIAN_POINT('Origin',(12.,3.4,10.));
#15962=CARTESIAN_POINT('Origin',(12.,2.5,10.));
#15963=CARTESIAN_POINT('',(10.2679491924311,2.5,11.));
#15964=CARTESIAN_POINT('',(10.2679491924311,3.4,11.));
#15965=CARTESIAN_POINT('',(10.2679491924311,2.5,11.));
#15966=CARTESIAN_POINT('',(10.2679491924311,2.5,9.));
#15967=CARTESIAN_POINT('Origin',(12.,2.5,10.));
#15968=CARTESIAN_POINT('',(10.2679491924311,3.4,9.));
#15969=CARTESIAN_POINT('',(10.2679491924311,2.5,9.));
#15970=CARTESIAN_POINT('Origin',(12.,3.4,10.));
#15971=CARTESIAN_POINT('Origin',(7.,3.4,10.));
#15972=CARTESIAN_POINT('',(3.73205080756888,3.4,9.));
#15973=CARTESIAN_POINT('',(2.,3.4,9.));
#15974=CARTESIAN_POINT('',(3.73205080756888,3.4,11.));
#15975=CARTESIAN_POINT('Origin',(2.,3.4,10.));
#15976=CARTESIAN_POINT('',(12.,3.4,11.));
#15977=CARTESIAN_POINT('Origin',(12.,2.5,9.));
#15978=CARTESIAN_POINT('',(3.73205080756888,2.5,9.));
#15979=CARTESIAN_POINT('',(2.,2.5,9.));
#15980=CARTESIAN_POINT('',(3.73205080756888,2.5,9.));
#15981=CARTESIAN_POINT('Origin',(2.,2.5,10.));
#15982=CARTESIAN_POINT('',(3.73205080756888,2.5,11.));
#15983=CARTESIAN_POINT('',(3.73205080756888,2.5,11.));
#15984=CARTESIAN_POINT('Origin',(2.,2.5,10.));
#15985=CARTESIAN_POINT('Origin',(2.,2.5,11.));
#15986=CARTESIAN_POINT('',(12.,2.5,11.));
#15987=CARTESIAN_POINT('Origin',(7.,2.5,10.));
#15988=CARTESIAN_POINT('',(0.,0.,0.));
#15989=CARTESIAN_POINT('Origin',(2.,2.3,10.));
#15990=CARTESIAN_POINT('',(0.9,2.5,10.));
#15991=CARTESIAN_POINT('Origin',(2.,2.5,10.));
#15992=CARTESIAN_POINT('',(0.9,2.3,10.));
#15993=CARTESIAN_POINT('',(0.9,2.3,10.));
#15994=CARTESIAN_POINT('Origin',(2.,2.3,10.));
#15995=CARTESIAN_POINT('Origin',(2.,2.3,10.));
#15996=CARTESIAN_POINT('',(0.,2.5,10.));
#15997=CARTESIAN_POINT('Origin',(2.,2.5,10.));
#15998=CARTESIAN_POINT('',(0.,2.3,10.));
#15999=CARTESIAN_POINT('',(0.,2.3,10.));
#16000=CARTESIAN_POINT('Origin',(2.,2.3,10.));
#16001=CARTESIAN_POINT('Origin',(2.,2.5,10.));
#16002=CARTESIAN_POINT('Origin',(2.,2.3,10.));
#16003=CARTESIAN_POINT('',(0.,0.,0.));
#16004=CARTESIAN_POINT('Origin',(2.,3.4,10.));
#16005=CARTESIAN_POINT('',(0.9,3.6,10.));
#16006=CARTESIAN_POINT('Origin',(2.,3.6,10.));
#16007=CARTESIAN_POINT('',(0.9,3.4,10.));
#16008=CARTESIAN_POINT('',(0.9,3.4,10.));
#16009=CARTESIAN_POINT('Origin',(2.,3.4,10.));
#16010=CARTESIAN_POINT('Origin',(2.,3.4,10.));
#16011=CARTESIAN_POINT('',(0.,3.6,10.));
#16012=CARTESIAN_POINT('Origin',(2.,3.6,10.));
#16013=CARTESIAN_POINT('',(0.,3.4,10.));
#16014=CARTESIAN_POINT('',(0.,3.4,10.));
#16015=CARTESIAN_POINT('Origin',(2.,3.4,10.));
#16016=CARTESIAN_POINT('Origin',(2.,3.6,10.));
#16017=CARTESIAN_POINT('Origin',(2.,3.4,10.));
#16018=CARTESIAN_POINT('',(0.,0.,0.));
#16019=CARTESIAN_POINT('Origin',(12.,2.3,10.));
#16020=CARTESIAN_POINT('',(10.9,2.5,10.));
#16021=CARTESIAN_POINT('Origin',(12.,2.5,10.));
#16022=CARTESIAN_POINT('',(10.9,2.3,10.));
#16023=CARTESIAN_POINT('',(10.9,2.3,10.));
#16024=CARTESIAN_POINT('Origin',(12.,2.3,10.));
#16025=CARTESIAN_POINT('Origin',(12.,2.3,10.));
#16026=CARTESIAN_POINT('',(10.,2.5,10.));
#16027=CARTESIAN_POINT('Origin',(12.,2.5,10.));
#16028=CARTESIAN_POINT('',(10.,2.3,10.));
#16029=CARTESIAN_POINT('',(10.,2.3,10.));
#16030=CARTESIAN_POINT('Origin',(12.,2.3,10.));
#16031=CARTESIAN_POINT('Origin',(12.,2.5,10.));
#16032=CARTESIAN_POINT('Origin',(12.,2.3,10.));
#16033=CARTESIAN_POINT('',(0.,0.,0.));
#16034=CARTESIAN_POINT('Origin',(12.,3.4,10.));
#16035=CARTESIAN_POINT('',(10.9,3.6,10.));
#16036=CARTESIAN_POINT('Origin',(12.,3.6,10.));
#16037=CARTESIAN_POINT('',(10.9,3.4,10.));
#16038=CARTESIAN_POINT('',(10.9,3.4,10.));
#16039=CARTESIAN_POINT('Origin',(12.,3.4,10.));
#16040=CARTESIAN_POINT('Origin',(12.,3.4,10.));
#16041=CARTESIAN_POINT('',(10.,3.6,10.));
#16042=CARTESIAN_POINT('Origin',(12.,3.6,10.));
#16043=CARTESIAN_POINT('',(10.,3.4,10.));
#16044=CARTESIAN_POINT('',(10.,3.4,10.));
#16045=CARTESIAN_POINT('Origin',(12.,3.4,10.));
#16046=CARTESIAN_POINT('Origin',(12.,3.6,10.));
#16047=CARTESIAN_POINT('Origin',(12.,3.4,10.));
#16048=CARTESIAN_POINT('',(0.,0.,0.));
#16049=CARTESIAN_POINT('',(0.,0.,0.));
#16050=CARTESIAN_POINT('Origin',(0.,0.,0.));
#16051=CARTESIAN_POINT('',(-0.976185,-0.246528389340863,-1.19548183562566E-16));
#16052=CARTESIAN_POINT('',(-1.19548183562566E-16,-0.246528389340863,0.976185));
#16053=CARTESIAN_POINT('Origin',(0.,-0.246528389340863,0.));
#16054=CARTESIAN_POINT('Origin',(0.,-0.246528389340863,0.));
#16055=CARTESIAN_POINT('',(-1.19548183562566E-16,0.246528389340863,0.976185));
#16056=CARTESIAN_POINT('Origin',(-1.22464679914735E-16,0.,1.));
#16057=CARTESIAN_POINT('',(-0.976185,0.246528389340863,1.19548183562566E-16));
#16058=CARTESIAN_POINT('Origin',(0.,0.246528389340863,0.));
#16059=CARTESIAN_POINT('Origin',(0.,0.246528389340863,0.));
#16060=CARTESIAN_POINT('Origin',(0.,0.,0.));
#16061=CARTESIAN_POINT('',(-0.976185,0.45,-1.19548183562566E-16));
#16062=CARTESIAN_POINT('',(-0.976185,0.,-1.19548183562566E-16));
#16063=CARTESIAN_POINT('Origin',(0.,0.45,0.));
#16064=CARTESIAN_POINT('Origin',(0.,0.,0.));
#16065=CARTESIAN_POINT('',(-0.5,-0.39,-6.12323399573677E-17));
#16066=CARTESIAN_POINT('Origin',(0.,-0.39,0.));
#16067=CARTESIAN_POINT('',(-0.5,0.39,-6.12323399573677E-17));
#16068=CARTESIAN_POINT('',(-0.5,0.,-6.12323399573677E-17));
#16069=CARTESIAN_POINT('Origin',(0.,0.39,0.));
#16070=CARTESIAN_POINT('Origin',(0.,0.42,0.));
#16071=CARTESIAN_POINT('',(-0.56,0.45,-6.85802207522518E-17));
#16072=CARTESIAN_POINT('',(-0.53,0.42,-6.49062803548097E-17));
#16073=CARTESIAN_POINT('Origin',(0.,0.45,0.));
#16074=CARTESIAN_POINT('Origin',(0.976185,0.45,0.));
#16075=CARTESIAN_POINT('Origin',(0.,0.,0.));
#16076=CARTESIAN_POINT('',(-0.976185,-0.45,-1.19548183562566E-16));
#16077=CARTESIAN_POINT('Origin',(0.,-0.45,0.));
#16078=CARTESIAN_POINT('',(-0.976185,0.,-1.19548183562566E-16));
#16079=CARTESIAN_POINT('Origin',(0.56,-0.45,0.));
#16080=CARTESIAN_POINT('',(-0.56,-0.45,-6.85802207522518E-17));
#16081=CARTESIAN_POINT('Origin',(0.,-0.45,0.));
#16082=CARTESIAN_POINT('Origin',(0.,-0.42,0.));
#16083=CARTESIAN_POINT('',(-0.53,-0.42,-6.49062803548097E-17));
#16084=CARTESIAN_POINT('',(0.,0.,0.));
#16085=CARTESIAN_POINT('Origin',(0.,0.,0.));
#16086=CARTESIAN_POINT('',(-1.023815,0.246528389340863,-1.25381176266905E-16));
#16087=CARTESIAN_POINT('',(-1.25381176266905E-16,0.246528389340863,1.023815));
#16088=CARTESIAN_POINT('Origin',(0.,0.246528389340863,0.));
#16089=CARTESIAN_POINT('Origin',(0.,0.246528389340863,0.));
#16090=CARTESIAN_POINT('',(-1.25381176266905E-16,-0.246528389340863,1.023815));
#16091=CARTESIAN_POINT('Origin',(-1.22464679914735E-16,0.,1.));
#16092=CARTESIAN_POINT('',(-1.023815,-0.246528389340863,1.25381176266905E-16));
#16093=CARTESIAN_POINT('Origin',(0.,-0.246528389340863,0.));
#16094=CARTESIAN_POINT('Origin',(0.,-0.246528389340863,0.));
#16095=CARTESIAN_POINT('Origin',(0.,0.,0.));
#16096=CARTESIAN_POINT('',(-1.023815,-0.45,-1.25381176266905E-16));
#16097=CARTESIAN_POINT('Origin',(0.,-0.45,0.));
#16098=CARTESIAN_POINT('',(-1.023815,0.,-1.25381176266905E-16));
#16099=CARTESIAN_POINT('Origin',(1.44,0.45,0.));
#16100=CARTESIAN_POINT('',(-1.44,0.45,-1.76349139077219E-16));
#16101=CARTESIAN_POINT('Origin',(0.,0.45,0.));
#16102=CARTESIAN_POINT('',(-1.023815,0.45,-1.25381176266905E-16));
#16103=CARTESIAN_POINT('Origin',(0.,0.45,0.));
#16104=CARTESIAN_POINT('Origin',(0.,0.42,0.));
#16105=CARTESIAN_POINT('',(-1.5,0.39,-1.83697019872103E-16));
#16106=CARTESIAN_POINT('Origin',(0.,0.39,0.));
#16107=CARTESIAN_POINT('',(-1.47,0.42,-1.80023079474661E-16));
#16108=CARTESIAN_POINT('Origin',(0.,0.,0.));
#16109=CARTESIAN_POINT('',(-1.5,-0.39,-1.83697019872103E-16));
#16110=CARTESIAN_POINT('Origin',(0.,-0.39,0.));
#16111=CARTESIAN_POINT('',(-1.5,0.,-1.83697019872103E-16));
#16112=CARTESIAN_POINT('Origin',(0.,-0.42,0.));
#16113=CARTESIAN_POINT('',(-1.44,-0.45,-1.76349139077219E-16));
#16114=CARTESIAN_POINT('Origin',(0.,-0.45,0.));
#16115=CARTESIAN_POINT('',(-1.47,-0.42,-1.80023079474661E-16));
#16116=CARTESIAN_POINT('Origin',(1.023815,-0.45,0.));
#16117=CARTESIAN_POINT('Origin',(0.,0.,0.));
#16118=CARTESIAN_POINT('',(-1.023815,0.,-1.25381176266905E-16));
#16119=CARTESIAN_POINT('',(0.,0.,0.));
#16120=CARTESIAN_POINT('Origin',(1.,0.,0.));
#16121=CARTESIAN_POINT('',(1.,-1.78583896120461E-33,0.23815));
#16122=CARTESIAN_POINT('',(1.,-1.78583896120461E-33,-0.23815));
#16123=CARTESIAN_POINT('Origin',(1.,0.,0.));
#16124=CARTESIAN_POINT('Origin',(0.707106781186548,0.,-0.707106781186547));
#16125=CARTESIAN_POINT('',(0.875504261126124,-1.78583896120461E-33,-0.538709301246971));
#16126=CARTESIAN_POINT('',(0.538709301246971,-1.78583896120461E-33,-0.875504261126124));
#16127=CARTESIAN_POINT('Origin',(0.707106781186548,0.,-0.707106781186547));
#16128=CARTESIAN_POINT('Origin',(6.12323399573677E-17,0.,-1.));
#16129=CARTESIAN_POINT('',(0.23815,-1.78583896120461E-33,-1.));
#16130=CARTESIAN_POINT('',(-0.23815,-1.78583896120461E-33,-1.));
#16131=CARTESIAN_POINT('Origin',(6.12323399573677E-17,0.,-1.));
#16132=CARTESIAN_POINT('Origin',(-0.707106781186547,0.,-0.707106781186548));
#16133=CARTESIAN_POINT('',(-0.538709301246971,-1.78583896120461E-33,-0.875504261126124));
#16134=CARTESIAN_POINT('',(-0.875504261126124,-1.78583896120461E-33,-0.538709301246971));
#16135=CARTESIAN_POINT('Origin',(-0.707106781186547,0.,-0.707106781186548));
#16136=CARTESIAN_POINT('Origin',(-1.,0.,-1.22464679914735E-16));
#16137=CARTESIAN_POINT('',(-1.,-1.78583896120461E-33,-0.23815));
#16138=CARTESIAN_POINT('',(-1.,-1.78583896120461E-33,0.23815));
#16139=CARTESIAN_POINT('Origin',(-1.,0.,-1.22464679914735E-16));
#16140=CARTESIAN_POINT('Origin',(-0.707106781186548,0.,0.707106781186547));
#16141=CARTESIAN_POINT('',(-0.875504261126124,-7.94881478324376E-33,0.538709301246971));
#16142=CARTESIAN_POINT('',(-0.538709301246971,4.37713686083455E-33,0.875504261126124));
#16143=CARTESIAN_POINT('Origin',(-0.707106781186548,0.,0.707106781186547));
#16144=CARTESIAN_POINT('Origin',(-1.83697019872103E-16,0.,1.));
#16145=CARTESIAN_POINT('',(-0.23815,-1.78583896120461E-33,1.));
#16146=CARTESIAN_POINT('',(0.23815,-1.78583896120461E-33,1.));
#16147=CARTESIAN_POINT('Origin',(-1.83697019872103E-16,0.,1.));
#16148=CARTESIAN_POINT('Origin',(0.707106781186547,0.,0.707106781186548));
#16149=CARTESIAN_POINT('',(0.538709301246971,-4.86732687222419E-33,0.875504261126124));
#16150=CARTESIAN_POINT('',(0.875504261126124,1.29564894981497E-33,0.538709301246971));
#16151=CARTESIAN_POINT('Origin',(0.707106781186547,0.,0.707106781186548));
#16152=CARTESIAN_POINT('',(0.,0.,0.));
#16153=CARTESIAN_POINT('Origin',(0.707106781186547,0.,0.707106781186548));
#16154=CARTESIAN_POINT('',(0.504455939115715,-0.04763,0.841298510752802));
#16155=CARTESIAN_POINT('',(0.841298510752802,-0.04763,0.504455939115715));
#16156=CARTESIAN_POINT('Ctrl Pts',(0.504455939115715,-0.04763,0.841298510752802));
#16157=CARTESIAN_POINT('Ctrl Pts',(0.508899795931835,-0.0740444353928835,
0.838633903678357));
#16158=CARTESIAN_POINT('Ctrl Pts',(0.517157748491652,-0.0999305678883309,
0.833661031856294));
#16159=CARTESIAN_POINT('Ctrl Pts',(0.537715343527944,-0.142345102874864,
0.820511285096538));
#16160=CARTESIAN_POINT('Ctrl Pts',(0.548874290046456,-0.159766064500479,
0.813159949759));
#16161=CARTESIAN_POINT('Ctrl Pts',(0.573915184558107,-0.190326085855194,
0.795684265985089));
#16162=CARTESIAN_POINT('Ctrl Pts',(0.587792702767295,-0.203463743702801,
0.78555112003688));
#16163=CARTESIAN_POINT('Ctrl Pts',(0.615966552324775,-0.224161999508995,
0.763642258217233));
#16164=CARTESIAN_POINT('Ctrl Pts',(0.631684198665438,-0.232861760990032,
0.750785745543687));
#16165=CARTESIAN_POINT('Ctrl Pts',(0.663382628119203,-0.244251601209411,
0.722929908501543));
#16166=CARTESIAN_POINT('Ctrl Pts',(0.679352081686668,-0.246942143572133,
0.707917883896095));
#16167=CARTESIAN_POINT('Ctrl Pts',(0.707917883896095,-0.246942143572133,
0.679352081686668));
#16168=CARTESIAN_POINT('Ctrl Pts',(0.722929908501543,-0.244251601209411,
0.663382628119203));
#16169=CARTESIAN_POINT('Ctrl Pts',(0.750785745543687,-0.232861760990032,
0.631684198665439));
#16170=CARTESIAN_POINT('Ctrl Pts',(0.763642258217232,-0.224161999508995,
0.615966552324775));
#16171=CARTESIAN_POINT('Ctrl Pts',(0.78555112003688,-0.203463743702801,
0.587792702767295));
#16172=CARTESIAN_POINT('Ctrl Pts',(0.795684265985088,-0.190326085855194,
0.573915184558108));
#16173=CARTESIAN_POINT('Ctrl Pts',(0.813159949759,-0.15976606450048,0.548874290046456));
#16174=CARTESIAN_POINT('Ctrl Pts',(0.820511285096538,-0.142345102874864,
0.537715343527944));
#16175=CARTESIAN_POINT('Ctrl Pts',(0.833661031856294,-0.099930567888331,
0.517157748491653));
#16176=CARTESIAN_POINT('Ctrl Pts',(0.838633903678357,-0.0740444353928835,
0.508899795931835));
#16177=CARTESIAN_POINT('Ctrl Pts',(0.841298510752801,-0.0476299999999999,
0.504455939115715));
#16178=CARTESIAN_POINT('',(0.528110872004958,-0.04763,0.871530771444223));
#16179=CARTESIAN_POINT('Origin',(0.707106781186547,-0.04763,0.707106781186548));
#16180=CARTESIAN_POINT('',(0.871530771444223,-0.04763,0.528110872004959));
#16181=CARTESIAN_POINT('Ctrl Pts',(0.871530771444223,-0.0476300000000001,
0.528110872004958));
#16182=CARTESIAN_POINT('Ctrl Pts',(0.87014664509073,-0.0609922781173483,
0.530395067942936));
#16183=CARTESIAN_POINT('Ctrl Pts',(0.868149331745851,-0.0742967091364493,
0.533674141594226));
#16184=CARTESIAN_POINT('Ctrl Pts',(0.85981294420286,-0.115492077056649,
0.54708917182331));
#16185=CARTESIAN_POINT('Ctrl Pts',(0.850993704737257,-0.141695629206859,
0.560922177770136));
#16186=CARTESIAN_POINT('Ctrl Pts',(0.830754510485543,-0.181890537957859,
0.590422647829571));
#16187=CARTESIAN_POINT('Ctrl Pts',(0.816896541396381,-0.201072148666545,
0.609616703125488));
#16188=CARTESIAN_POINT('Ctrl Pts',(0.792310597819928,-0.223955109275652,
0.641117951819998));
#16189=CARTESIAN_POINT('Ctrl Pts',(0.779109323683612,-0.232742381310829,
0.657208095763053));
#16190=CARTESIAN_POINT('Ctrl Pts',(0.750552691816206,-0.244234834628584,
0.68964083160521));
#16191=CARTESIAN_POINT('Ctrl Pts',(0.735185187071673,-0.246942143572133,
0.705971972091755));
#16192=CARTESIAN_POINT('Ctrl Pts',(0.705971972091754,-0.246942143572133,
0.735185187071673));
#16193=CARTESIAN_POINT('Ctrl Pts',(0.689640831605209,-0.244234834628584,
0.750552691816206));
#16194=CARTESIAN_POINT('Ctrl Pts',(0.657208095763052,-0.232742381310829,
0.779109323683612));
#16195=CARTESIAN_POINT('Ctrl Pts',(0.641117951819998,-0.223955109275652,
0.792310597819928));
#16196=CARTESIAN_POINT('Ctrl Pts',(0.609616703125487,-0.201072148666545,
0.816896541396382));
#16197=CARTESIAN_POINT('Ctrl Pts',(0.590422647829571,-0.181890537957858,
0.830754510485544));
#16198=CARTESIAN_POINT('Ctrl Pts',(0.560922177770135,-0.141695629206858,
0.850993704737257));
#16199=CARTESIAN_POINT('Ctrl Pts',(0.547089171823309,-0.115492077056649,
0.859812944202861));
#16200=CARTESIAN_POINT('Ctrl Pts',(0.533674141594226,-0.0742967091364491,
0.868149331745852));
#16201=CARTESIAN_POINT('Ctrl Pts',(0.530395067942936,-0.0609922781173483,
0.870146645090731));
#16202=CARTESIAN_POINT('Ctrl Pts',(0.528110872004958,-0.0476300000000001,
0.871530771444223));
#16203=CARTESIAN_POINT('Origin',(0.707106781186547,-0.04763,0.707106781186548));
#16204=CARTESIAN_POINT('Origin',(0.,-0.166705,0.));
#16205=CARTESIAN_POINT('',(0.242834539687906,-0.04763,0.989696097314));
#16206=CARTESIAN_POINT('Origin',(0.,-0.04763,0.));
#16207=CARTESIAN_POINT('',(-0.242834539687907,-0.04763,0.989696097314));
#16208=CARTESIAN_POINT('Ctrl Pts',(0.242834539687906,-0.04763,0.989696097314));
#16209=CARTESIAN_POINT('Ctrl Pts',(0.24024064412003,-0.0609922781173483,
0.990332542620729));
#16210=CARTESIAN_POINT('Ctrl Pts',(0.236509675094874,-0.0742967091364492,
0.991238884025248));
#16211=CARTESIAN_POINT('Ctrl Pts',(0.221129100087819,-0.115492077056649,
0.994830026707808));
#16212=CARTESIAN_POINT('Ctrl Pts',(0.205111543747588,-0.141695629206859,
0.998375294985966));
#16213=CARTESIAN_POINT('Ctrl Pts',(0.169940289819232,-0.181890537957859,
1.00492400591205));
#16214=CARTESIAN_POINT('Ctrl Pts',(0.1465689792446,-0.201072148666545,1.00869718865384));
#16215=CARTESIAN_POINT('Ctrl Pts',(0.106909345252087,-0.223955109275652,
1.01358704779679));
#16216=CARTESIAN_POINT('Ctrl Pts',(0.0861971848975941,-0.232742381310829,
1.0156297872271));
#16217=CARTESIAN_POINT('Ctrl Pts',(0.0430711894098822,-0.244234834628584,
1.01837060663223));
#16218=CARTESIAN_POINT('Ctrl Pts',(0.0206568624125605,-0.246942143572133,
1.019052));
#16219=CARTESIAN_POINT('Ctrl Pts',(-0.0206568624125608,-0.246942143572133,
1.019052));
#16220=CARTESIAN_POINT('Ctrl Pts',(-0.0430711894098825,-0.244234834628584,
1.01837060663223));
#16221=CARTESIAN_POINT('Ctrl Pts',(-0.0861971848975943,-0.232742381310829,
1.0156297872271));
#16222=CARTESIAN_POINT('Ctrl Pts',(-0.106909345252088,-0.223955109275652,
1.01358704779679));
#16223=CARTESIAN_POINT('Ctrl Pts',(-0.1465689792446,-0.201072148666545,
1.00869718865384));
#16224=CARTESIAN_POINT('Ctrl Pts',(-0.169940289819232,-0.181890537957859,
1.00492400591205));
#16225=CARTESIAN_POINT('Ctrl Pts',(-0.205111543747588,-0.141695629206859,
0.998375294985966));
#16226=CARTESIAN_POINT('Ctrl Pts',(-0.221129100087819,-0.115492077056649,
0.994830026707808));
#16227=CARTESIAN_POINT('Ctrl Pts',(-0.236509675094875,-0.0742967091364493,
0.991238884025248));
#16228=CARTESIAN_POINT('Ctrl Pts',(-0.24024064412003,-0.0609922781173483,
0.990332542620729));
#16229=CARTESIAN_POINT('Ctrl Pts',(-0.242834539687907,-0.04763,0.989696097314));
#16230=CARTESIAN_POINT('',(-0.528110872004959,-0.04763,0.871530771444223));
#16231=CARTESIAN_POINT('Origin',(0.,-0.04763,0.));
#16232=CARTESIAN_POINT('',(-0.871530771444223,-0.04763,0.528110872004958));
#16233=CARTESIAN_POINT('Ctrl Pts',(-0.528110872004958,-0.0476300000000001,
0.871530771444223));
#16234=CARTESIAN_POINT('Ctrl Pts',(-0.530395067942936,-0.0609922781173484,
0.87014664509073));
#16235=CARTESIAN_POINT('Ctrl Pts',(-0.533674141594226,-0.0742967091364493,
0.868149331745851));
#16236=CARTESIAN_POINT('Ctrl Pts',(-0.54708917182331,-0.115492077056649,
0.85981294420286));
#16237=CARTESIAN_POINT('Ctrl Pts',(-0.560922177770136,-0.141695629206859,
0.850993704737257));
#16238=CARTESIAN_POINT('Ctrl Pts',(-0.590422647829571,-0.181890537957859,
0.830754510485543));
#16239=CARTESIAN_POINT('Ctrl Pts',(-0.609616703125488,-0.201072148666545,
0.816896541396381));
#16240=CARTESIAN_POINT('Ctrl Pts',(-0.641117951819998,-0.223955109275652,
0.792310597819928));
#16241=CARTESIAN_POINT('Ctrl Pts',(-0.657208095763053,-0.232742381310829,
0.779109323683611));
#16242=CARTESIAN_POINT('Ctrl Pts',(-0.68964083160521,-0.244234834628584,
0.750552691816205));
#16243=CARTESIAN_POINT('Ctrl Pts',(-0.705971972091755,-0.246942143572133,
0.735185187071673));
#16244=CARTESIAN_POINT('Ctrl Pts',(-0.735185187071673,-0.246942143572133,
0.705971972091754));
#16245=CARTESIAN_POINT('Ctrl Pts',(-0.750552691816206,-0.244234834628584,
0.689640831605209));
#16246=CARTESIAN_POINT('Ctrl Pts',(-0.779109323683612,-0.232742381310829,
0.657208095763052));
#16247=CARTESIAN_POINT('Ctrl Pts',(-0.792310597819928,-0.223955109275652,
0.641117951819998));
#16248=CARTESIAN_POINT('Ctrl Pts',(-0.816896541396382,-0.201072148666545,
0.609616703125487));
#16249=CARTESIAN_POINT('Ctrl Pts',(-0.830754510485544,-0.181890537957858,
0.590422647829571));
#16250=CARTESIAN_POINT('Ctrl Pts',(-0.850993704737257,-0.141695629206858,
0.560922177770135));
#16251=CARTESIAN_POINT('Ctrl Pts',(-0.859812944202861,-0.115492077056649,
0.547089171823309));
#16252=CARTESIAN_POINT('Ctrl Pts',(-0.868149331745852,-0.0742967091364491,
0.533674141594226));
#16253=CARTESIAN_POINT('Ctrl Pts',(-0.870146645090731,-0.0609922781173483,
0.530395067942936));
#16254=CARTESIAN_POINT('Ctrl Pts',(-0.871530771444223,-0.04763,0.528110872004958));
#16255=CARTESIAN_POINT('',(-0.989696097314,-0.04763,0.242834539687906));
#16256=CARTESIAN_POINT('Origin',(0.,-0.04763,0.));
#16257=CARTESIAN_POINT('',(-1.019052,-0.246942143572133,1.248489836334E-16));
#16258=CARTESIAN_POINT('Ctrl Pts',(-0.989696097314,-0.04763,0.242834539687906));
#16259=CARTESIAN_POINT('Ctrl Pts',(-0.990332542620729,-0.0609922781173483,
0.24024064412003));
#16260=CARTESIAN_POINT('Ctrl Pts',(-0.991238884025248,-0.0742967091364492,
0.236509675094874));
#16261=CARTESIAN_POINT('Ctrl Pts',(-0.994830026707808,-0.115492077056649,
0.221129100087819));
#16262=CARTESIAN_POINT('Ctrl Pts',(-0.998375294985966,-0.141695629206859,
0.205111543747588));
#16263=CARTESIAN_POINT('Ctrl Pts',(-1.00492400591205,-0.181890537957859,
0.169940289819232));
#16264=CARTESIAN_POINT('Ctrl Pts',(-1.00869718865384,-0.201072148666545,
0.1465689792446));
#16265=CARTESIAN_POINT('Ctrl Pts',(-1.01358704779679,-0.223955109275652,
0.106909345252088));
#16266=CARTESIAN_POINT('Ctrl Pts',(-1.0156297872271,-0.232742381310829,
0.0861971848975944));
#16267=CARTESIAN_POINT('Ctrl Pts',(-1.01837060663223,-0.244234834628584,
0.0430711894098825));
#16268=CARTESIAN_POINT('Ctrl Pts',(-1.019052,-0.246942143572133,0.0206568624125608));
#16269=CARTESIAN_POINT('Ctrl Pts',(-1.019052,-0.246942143572133,1.2490009027033E-16));
#16270=CARTESIAN_POINT('',(-1.019052,-0.28578,1.24797876996471E-16));
#16271=CARTESIAN_POINT('',(-1.019052,-0.166705,1.24797876996471E-16));
#16272=CARTESIAN_POINT('Origin',(0.,-0.28578,0.));
#16273=CARTESIAN_POINT('',(-0.989696097314,-0.04763,-0.242834539687906));
#16274=CARTESIAN_POINT('Ctrl Pts',(-1.019052,-0.246942143572133,1.2490009027033E-16));
#16275=CARTESIAN_POINT('Ctrl Pts',(-1.019052,-0.246942143572133,-0.0206568624125605));
#16276=CARTESIAN_POINT('Ctrl Pts',(-1.01837060663223,-0.244234834628584,
-0.0430711894098822));
#16277=CARTESIAN_POINT('Ctrl Pts',(-1.0156297872271,-0.232742381310829,
-0.0861971848975941));
#16278=CARTESIAN_POINT('Ctrl Pts',(-1.01358704779679,-0.223955109275652,
-0.106909345252087));
#16279=CARTESIAN_POINT('Ctrl Pts',(-1.00869718865384,-0.201072148666546,
-0.1465689792446));
#16280=CARTESIAN_POINT('Ctrl Pts',(-1.00492400591205,-0.181890537957859,
-0.169940289819232));
#16281=CARTESIAN_POINT('Ctrl Pts',(-0.998375294985966,-0.141695629206859,
-0.205111543747588));
#16282=CARTESIAN_POINT('Ctrl Pts',(-0.994830026707808,-0.11549207705665,
-0.221129100087819));
#16283=CARTESIAN_POINT('Ctrl Pts',(-0.991238884025248,-0.0742967091364495,
-0.236509675094874));
#16284=CARTESIAN_POINT('Ctrl Pts',(-0.990332542620729,-0.0609922781173484,
-0.24024064412003));
#16285=CARTESIAN_POINT('Ctrl Pts',(-0.989696097314,-0.0476300000000001,
-0.242834539687907));
#16286=CARTESIAN_POINT('',(-0.871530771444223,-0.04763,-0.528110872004958));
#16287=CARTESIAN_POINT('Origin',(0.,-0.04763,0.));
#16288=CARTESIAN_POINT('',(-0.528110872004958,-0.04763,-0.871530771444223));
#16289=CARTESIAN_POINT('Ctrl Pts',(-0.871530771444223,-0.0476300000000001,
-0.528110872004958));
#16290=CARTESIAN_POINT('Ctrl Pts',(-0.87014664509073,-0.0609922781173484,
-0.530395067942936));
#16291=CARTESIAN_POINT('Ctrl Pts',(-0.868149331745851,-0.0742967091364494,
-0.533674141594226));
#16292=CARTESIAN_POINT('Ctrl Pts',(-0.85981294420286,-0.115492077056649,
-0.54708917182331));
#16293=CARTESIAN_POINT('Ctrl Pts',(-0.850993704737257,-0.141695629206859,
-0.560922177770136));
#16294=CARTESIAN_POINT('Ctrl Pts',(-0.830754510485543,-0.181890537957859,
-0.590422647829571));
#16295=CARTESIAN_POINT('Ctrl Pts',(-0.816896541396381,-0.201072148666546,
-0.609616703125488));
#16296=CARTESIAN_POINT('Ctrl Pts',(-0.792310597819928,-0.223955109275652,
-0.641117951819999));
#16297=CARTESIAN_POINT('Ctrl Pts',(-0.779109323683611,-0.232742381310829,
-0.657208095763053));
#16298=CARTESIAN_POINT('Ctrl Pts',(-0.750552691816205,-0.244234834628584,
-0.68964083160521));
#16299=CARTESIAN_POINT('Ctrl Pts',(-0.735185187071673,-0.246942143572133,
-0.705971972091755));
#16300=CARTESIAN_POINT('Ctrl Pts',(-0.705971972091754,-0.246942143572133,
-0.735185187071673));
#16301=CARTESIAN_POINT('Ctrl Pts',(-0.68964083160521,-0.244234834628584,
-0.750552691816206));
#16302=CARTESIAN_POINT('Ctrl Pts',(-0.657208095763052,-0.232742381310829,
-0.779109323683612));
#16303=CARTESIAN_POINT('Ctrl Pts',(-0.641117951819998,-0.223955109275652,
-0.792310597819928));
#16304=CARTESIAN_POINT('Ctrl Pts',(-0.609616703125488,-0.201072148666545,
-0.816896541396381));
#16305=CARTESIAN_POINT('Ctrl Pts',(-0.590422647829571,-0.181890537957859,
-0.830754510485543));
#16306=CARTESIAN_POINT('Ctrl Pts',(-0.560922177770136,-0.141695629206859,
-0.850993704737257));
#16307=CARTESIAN_POINT('Ctrl Pts',(-0.54708917182331,-0.115492077056649,
-0.85981294420286));
#16308=CARTESIAN_POINT('Ctrl Pts',(-0.533674141594226,-0.0742967091364494,
-0.868149331745852));
#16309=CARTESIAN_POINT('Ctrl Pts',(-0.530395067942936,-0.0609922781173484,
-0.870146645090731));
#16310=CARTESIAN_POINT('Ctrl Pts',(-0.528110872004958,-0.0476300000000001,
-0.871530771444223));
#16311=CARTESIAN_POINT('',(-0.242834539687906,-0.04763,-0.989696097314));
#16312=CARTESIAN_POINT('Origin',(0.,-0.04763,0.));
#16313=CARTESIAN_POINT('',(0.242834539687906,-0.04763,-0.989696097314));
#16314=CARTESIAN_POINT('Ctrl Pts',(-0.242834539687907,-0.04763,-0.989696097314));
#16315=CARTESIAN_POINT('Ctrl Pts',(-0.24024064412003,-0.0609922781173483,
-0.990332542620729));
#16316=CARTESIAN_POINT('Ctrl Pts',(-0.236509675094874,-0.0742967091364493,
-0.991238884025248));
#16317=CARTESIAN_POINT('Ctrl Pts',(-0.221129100087819,-0.115492077056649,
-0.994830026707808));
#16318=CARTESIAN_POINT('Ctrl Pts',(-0.205111543747588,-0.141695629206859,
-0.998375294985966));
#16319=CARTESIAN_POINT('Ctrl Pts',(-0.169940289819232,-0.181890537957859,
-1.00492400591205));
#16320=CARTESIAN_POINT('Ctrl Pts',(-0.1465689792446,-0.201072148666545,
-1.00869718865384));
#16321=CARTESIAN_POINT('Ctrl Pts',(-0.106909345252087,-0.223955109275652,
-1.01358704779679));
#16322=CARTESIAN_POINT('Ctrl Pts',(-0.0861971848975942,-0.232742381310829,
-1.0156297872271));
#16323=CARTESIAN_POINT('Ctrl Pts',(-0.0430711894098823,-0.244234834628584,
-1.01837060663223));
#16324=CARTESIAN_POINT('Ctrl Pts',(-0.0206568624125606,-0.246942143572133,
-1.019052));
#16325=CARTESIAN_POINT('Ctrl Pts',(0.0206568624125607,-0.246942143572133,
-1.019052));
#16326=CARTESIAN_POINT('Ctrl Pts',(0.0430711894098824,-0.244234834628584,
-1.01837060663223));
#16327=CARTESIAN_POINT('Ctrl Pts',(0.0861971848975943,-0.232742381310829,
-1.0156297872271));
#16328=CARTESIAN_POINT('Ctrl Pts',(0.106909345252088,-0.223955109275652,
-1.01358704779679));
#16329=CARTESIAN_POINT('Ctrl Pts',(0.1465689792446,-0.201072148666545,-1.00869718865384));
#16330=CARTESIAN_POINT('Ctrl Pts',(0.169940289819232,-0.181890537957859,
-1.00492400591205));
#16331=CARTESIAN_POINT('Ctrl Pts',(0.205111543747588,-0.141695629206859,
-0.998375294985966));
#16332=CARTESIAN_POINT('Ctrl Pts',(0.221129100087819,-0.115492077056649,
-0.994830026707808));
#16333=CARTESIAN_POINT('Ctrl Pts',(0.236509675094874,-0.0742967091364493,
-0.991238884025248));
#16334=CARTESIAN_POINT('Ctrl Pts',(0.24024064412003,-0.0609922781173484,
-0.990332542620729));
#16335=CARTESIAN_POINT('Ctrl Pts',(0.242834539687907,-0.04763,-0.989696097314));
#16336=CARTESIAN_POINT('',(0.528110872004958,-0.04763,-0.871530771444223));
#16337=CARTESIAN_POINT('Origin',(0.,-0.04763,0.));
#16338=CARTESIAN_POINT('',(0.871530771444223,-0.04763,-0.528110872004958));
#16339=CARTESIAN_POINT('Ctrl Pts',(0.528110872004958,-0.0476300000000001,
-0.871530771444223));
#16340=CARTESIAN_POINT('Ctrl Pts',(0.530395067942936,-0.0609922781173484,
-0.870146645090731));
#16341=CARTESIAN_POINT('Ctrl Pts',(0.533674141594226,-0.0742967091364493,
-0.868149331745851));
#16342=CARTESIAN_POINT('Ctrl Pts',(0.54708917182331,-0.115492077056649,
-0.85981294420286));
#16343=CARTESIAN_POINT('Ctrl Pts',(0.560922177770136,-0.141695629206859,
-0.850993704737257));
#16344=CARTESIAN_POINT('Ctrl Pts',(0.590422647829571,-0.181890537957859,
-0.830754510485543));
#16345=CARTESIAN_POINT('Ctrl Pts',(0.609616703125488,-0.201072148666545,
-0.816896541396381));
#16346=CARTESIAN_POINT('Ctrl Pts',(0.641117951819998,-0.223955109275652,
-0.792310597819928));
#16347=CARTESIAN_POINT('Ctrl Pts',(0.657208095763053,-0.232742381310829,
-0.779109323683612));
#16348=CARTESIAN_POINT('Ctrl Pts',(0.68964083160521,-0.244234834628584,
-0.750552691816206));
#16349=CARTESIAN_POINT('Ctrl Pts',(0.705971972091755,-0.246942143572133,
-0.735185187071673));
#16350=CARTESIAN_POINT('Ctrl Pts',(0.735185187071673,-0.246942143572133,
-0.705971972091754));
#16351=CARTESIAN_POINT('Ctrl Pts',(0.750552691816206,-0.244234834628584,
-0.68964083160521));
#16352=CARTESIAN_POINT('Ctrl Pts',(0.779109323683612,-0.232742381310829,
-0.657208095763053));
#16353=CARTESIAN_POINT('Ctrl Pts',(0.792310597819928,-0.223955109275652,
-0.641117951819998));
#16354=CARTESIAN_POINT('Ctrl Pts',(0.816896541396381,-0.201072148666545,
-0.609616703125488));
#16355=CARTESIAN_POINT('Ctrl Pts',(0.830754510485543,-0.181890537957859,
-0.590422647829571));
#16356=CARTESIAN_POINT('Ctrl Pts',(0.850993704737257,-0.141695629206859,
-0.560922177770136));
#16357=CARTESIAN_POINT('Ctrl Pts',(0.85981294420286,-0.115492077056649,
-0.54708917182331));
#16358=CARTESIAN_POINT('Ctrl Pts',(0.868149331745851,-0.0742967091364493,
-0.533674141594226));
#16359=CARTESIAN_POINT('Ctrl Pts',(0.870146645090731,-0.0609922781173484,
-0.530395067942936));
#16360=CARTESIAN_POINT('Ctrl Pts',(0.871530771444223,-0.0476300000000001,
-0.528110872004958));
#16361=CARTESIAN_POINT('',(0.989696097314,-0.04763,-0.242834539687906));
#16362=CARTESIAN_POINT('Origin',(0.,-0.04763,0.));
#16363=CARTESIAN_POINT('',(0.989696097314,-0.04763,0.242834539687906));
#16364=CARTESIAN_POINT('Ctrl Pts',(0.989696097314,-0.04763,-0.242834539687907));
#16365=CARTESIAN_POINT('Ctrl Pts',(0.990332542620729,-0.0609922781173483,
-0.24024064412003));
#16366=CARTESIAN_POINT('Ctrl Pts',(0.991238884025248,-0.0742967091364493,
-0.236509675094874));
#16367=CARTESIAN_POINT('Ctrl Pts',(0.994830026707808,-0.115492077056649,
-0.221129100087819));
#16368=CARTESIAN_POINT('Ctrl Pts',(0.998375294985966,-0.141695629206859,
-0.205111543747588));
#16369=CARTESIAN_POINT('Ctrl Pts',(1.00492400591205,-0.181890537957859,
-0.169940289819232));
#16370=CARTESIAN_POINT('Ctrl Pts',(1.00869718865384,-0.201072148666545,
-0.1465689792446));
#16371=CARTESIAN_POINT('Ctrl Pts',(1.01358704779679,-0.223955109275652,
-0.106909345252087));
#16372=CARTESIAN_POINT('Ctrl Pts',(1.0156297872271,-0.232742381310829,-0.0861971848975942));
#16373=CARTESIAN_POINT('Ctrl Pts',(1.01837060663223,-0.244234834628584,
-0.0430711894098823));
#16374=CARTESIAN_POINT('Ctrl Pts',(1.019052,-0.246942143572133,-0.0206568624125607));
#16375=CARTESIAN_POINT('Ctrl Pts',(1.019052,-0.246942143572133,0.0206568624125607));
#16376=CARTESIAN_POINT('Ctrl Pts',(1.01837060663223,-0.244234834628584,
0.0430711894098823));
#16377=CARTESIAN_POINT('Ctrl Pts',(1.0156297872271,-0.232742381310829,0.0861971848975942));
#16378=CARTESIAN_POINT('Ctrl Pts',(1.01358704779679,-0.223955109275652,
0.106909345252087));
#16379=CARTESIAN_POINT('Ctrl Pts',(1.00869718865384,-0.201072148666545,
0.1465689792446));
#16380=CARTESIAN_POINT('Ctrl Pts',(1.00492400591205,-0.181890537957859,
0.169940289819232));
#16381=CARTESIAN_POINT('Ctrl Pts',(0.998375294985966,-0.141695629206859,
0.205111543747588));
#16382=CARTESIAN_POINT('Ctrl Pts',(0.994830026707808,-0.115492077056649,
0.221129100087819));
#16383=CARTESIAN_POINT('Ctrl Pts',(0.991238884025248,-0.0742967091364492,
0.236509675094874));
#16384=CARTESIAN_POINT('Ctrl Pts',(0.990332542620729,-0.0609922781173483,
0.24024064412003));
#16385=CARTESIAN_POINT('Ctrl Pts',(0.989696097314,-0.04763,0.242834539687907));
#16386=CARTESIAN_POINT('Origin',(0.,-0.04763,0.));
#16387=CARTESIAN_POINT('Origin',(0.,-0.04763,0.));
#16388=CARTESIAN_POINT('',(0.238183666596899,-0.04763,0.951592097314));
#16389=CARTESIAN_POINT('Origin',(0.,-0.04763,0.));
#16390=CARTESIAN_POINT('Origin',(-1.94289029309402E-16,-0.04763,1.));
#16391=CARTESIAN_POINT('Origin',(-1.94289029309402E-16,0.,1.));
#16392=CARTESIAN_POINT('',(-0.2381836665969,-0.04763,0.951592097314));
#16393=CARTESIAN_POINT('Ctrl Pts',(-0.238183666596899,-0.0476299999999999,
0.951592097314));
#16394=CARTESIAN_POINT('Ctrl Pts',(-0.233157223576062,-0.0740444353928835,
0.952850216871763));
#16395=CARTESIAN_POINT('Ctrl Pts',(-0.223801617934946,-0.0999305678883309,
0.955173119738174));
#16396=CARTESIAN_POINT('Ctrl Pts',(-0.199966927975188,-0.142345102874864,
0.960411259488514));
#16397=CARTESIAN_POINT('Ctrl Pts',(-0.1868781821531,-0.159766064500479,
0.963103647174702));
#16398=CARTESIAN_POINT('Ctrl Pts',(-0.15681442133453,-0.190326085855194,
0.968453058988463));
#16399=CARTESIAN_POINT('Ctrl Pts',(-0.139836317888043,-0.203463743702801,
0.971100730005489));
#16400=CARTESIAN_POINT('Ctrl Pts',(-0.104422493053067,-0.224161999508995,
0.975530745318961));
#16401=CARTESIAN_POINT('Ctrl Pts',(-0.0842175114474176,-0.232861760990032,
0.977553872336861));
#16402=CARTESIAN_POINT('Ctrl Pts',(-0.0421062857595701,-0.244251601209411,
0.980270995488453));
#16403=CARTESIAN_POINT('Ctrl Pts',(-0.0201990724523197,-0.246942143572133,
0.980948));
#16404=CARTESIAN_POINT('Ctrl Pts',(0.020199072452319,-0.246942143572133,
0.980948));
#16405=CARTESIAN_POINT('Ctrl Pts',(0.0421062857595694,-0.244251601209411,
0.980270995488454));
#16406=CARTESIAN_POINT('Ctrl Pts',(0.0842175114474169,-0.232861760990032,
0.977553872336861));
#16407=CARTESIAN_POINT('Ctrl Pts',(0.104422493053067,-0.224161999508995,
0.975530745318961));
#16408=CARTESIAN_POINT('Ctrl Pts',(0.139836317888042,-0.203463743702801,
0.971100730005489));
#16409=CARTESIAN_POINT('Ctrl Pts',(0.15681442133453,-0.190326085855194,
0.968453058988463));
#16410=CARTESIAN_POINT('Ctrl Pts',(0.1868781821531,-0.15976606450048,0.963103647174702));
#16411=CARTESIAN_POINT('Ctrl Pts',(0.199966927975188,-0.142345102874864,
0.960411259488514));
#16412=CARTESIAN_POINT('Ctrl Pts',(0.223801617934945,-0.0999305678883309,
0.955173119738174));
#16413=CARTESIAN_POINT('Ctrl Pts',(0.233157223576061,-0.0740444353928835,
0.952850216871763));
#16414=CARTESIAN_POINT('Ctrl Pts',(0.238183666596899,-0.0476299999999999,
0.951592097314));
#16415=CARTESIAN_POINT('Origin',(-1.94289029309402E-16,-0.04763,1.));
#16416=CARTESIAN_POINT('Origin',(0.,-0.04763,0.));
#16417=CARTESIAN_POINT('',(-0.504455939115715,-0.04763,0.841298510752802));
#16418=CARTESIAN_POINT('Origin',(0.,-0.04763,0.));
#16419=CARTESIAN_POINT('Origin',(-0.707106781186548,-0.04763,0.707106781186547));
#16420=CARTESIAN_POINT('Origin',(-0.707106781186548,0.,0.707106781186547));
#16421=CARTESIAN_POINT('',(-0.841298510752802,-0.04763,0.504455939115715));
#16422=CARTESIAN_POINT('Ctrl Pts',(-0.841298510752802,-0.04763,0.504455939115715));
#16423=CARTESIAN_POINT('Ctrl Pts',(-0.838633903678357,-0.0740444353928835,
0.508899795931835));
#16424=CARTESIAN_POINT('Ctrl Pts',(-0.833661031856294,-0.0999305678883309,
0.517157748491652));
#16425=CARTESIAN_POINT('Ctrl Pts',(-0.820511285096538,-0.142345102874864,
0.537715343527944));
#16426=CARTESIAN_POINT('Ctrl Pts',(-0.813159949759,-0.159766064500479,0.548874290046456));
#16427=CARTESIAN_POINT('Ctrl Pts',(-0.795684265985089,-0.190326085855194,
0.573915184558107));
#16428=CARTESIAN_POINT('Ctrl Pts',(-0.78555112003688,-0.203463743702801,
0.587792702767295));
#16429=CARTESIAN_POINT('Ctrl Pts',(-0.763642258217233,-0.224161999508995,
0.615966552324775));
#16430=CARTESIAN_POINT('Ctrl Pts',(-0.750785745543687,-0.232861760990032,
0.631684198665438));
#16431=CARTESIAN_POINT('Ctrl Pts',(-0.722929908501543,-0.244251601209411,
0.663382628119203));
#16432=CARTESIAN_POINT('Ctrl Pts',(-0.707917883896095,-0.246942143572133,
0.679352081686668));
#16433=CARTESIAN_POINT('Ctrl Pts',(-0.679352081686668,-0.246942143572133,
0.707917883896095));
#16434=CARTESIAN_POINT('Ctrl Pts',(-0.663382628119203,-0.244251601209411,
0.722929908501544));
#16435=CARTESIAN_POINT('Ctrl Pts',(-0.631684198665438,-0.232861760990031,
0.750785745543687));
#16436=CARTESIAN_POINT('Ctrl Pts',(-0.615966552324775,-0.224161999508995,
0.763642258217233));
#16437=CARTESIAN_POINT('Ctrl Pts',(-0.587792702767295,-0.203463743702801,
0.78555112003688));
#16438=CARTESIAN_POINT('Ctrl Pts',(-0.573915184558107,-0.190326085855194,
0.795684265985088));
#16439=CARTESIAN_POINT('Ctrl Pts',(-0.548874290046456,-0.159766064500479,
0.813159949759));
#16440=CARTESIAN_POINT('Ctrl Pts',(-0.537715343527944,-0.142345102874864,
0.820511285096538));
#16441=CARTESIAN_POINT('Ctrl Pts',(-0.517157748491652,-0.0999305678883309,
0.833661031856294));
#16442=CARTESIAN_POINT('Ctrl Pts',(-0.508899795931835,-0.0740444353928835,
0.838633903678357));
#16443=CARTESIAN_POINT('Ctrl Pts',(-0.504455939115716,-0.04763,0.841298510752801));
#16444=CARTESIAN_POINT('Origin',(-0.707106781186548,-0.04763,0.707106781186547));
#16445=CARTESIAN_POINT('Origin',(0.,-0.04763,0.));
#16446=CARTESIAN_POINT('',(-0.951592097314,-0.04763,0.238183666596899));
#16447=CARTESIAN_POINT('Origin',(0.,-0.04763,0.));
#16448=CARTESIAN_POINT('Origin',(-1.,-0.04763,-1.11022302462516E-16));
#16449=CARTESIAN_POINT('Origin',(-1.,0.,-1.11022302462516E-16));
#16450=CARTESIAN_POINT('',(-0.951592097314,-0.04763,-0.2381836665969));
#16451=CARTESIAN_POINT('',(-0.980948,-0.246942143572133,1.08514323328844E-18));
#16452=CARTESIAN_POINT('Ctrl Pts',(-0.951592097314,-0.04763,-0.238183666596899));
#16453=CARTESIAN_POINT('Ctrl Pts',(-0.952850216871763,-0.0740444353928835,
-0.233157223576062));
#16454=CARTESIAN_POINT('Ctrl Pts',(-0.955173119738174,-0.0999305678883309,
-0.223801617934946));
#16455=CARTESIAN_POINT('Ctrl Pts',(-0.960411259488514,-0.142345102874864,
-0.199966927975188));
#16456=CARTESIAN_POINT('Ctrl Pts',(-0.963103647174702,-0.159766064500479,
-0.1868781821531));
#16457=CARTESIAN_POINT('Ctrl Pts',(-0.968453058988463,-0.190326085855194,
-0.15681442133453));
#16458=CARTESIAN_POINT('Ctrl Pts',(-0.971100730005489,-0.203463743702801,
-0.139836317888043));
#16459=CARTESIAN_POINT('Ctrl Pts',(-0.975530745318961,-0.224161999508995,
-0.104422493053067));
#16460=CARTESIAN_POINT('Ctrl Pts',(-0.977553872336861,-0.232861760990032,
-0.0842175114474175));
#16461=CARTESIAN_POINT('Ctrl Pts',(-0.980270995488453,-0.244251601209411,
-0.0421062857595699));
#16462=CARTESIAN_POINT('Ctrl Pts',(-0.980948,-0.246942143572133,-0.0201990724523195));
#16463=CARTESIAN_POINT('Ctrl Pts',(-0.980948,-0.246942143572133,-1.17961196366423E-16));
#16464=CARTESIAN_POINT('Origin',(-1.,-0.04763,-1.11022302462516E-16));
#16465=CARTESIAN_POINT('Ctrl Pts',(-0.980948,-0.246942143572133,-1.17961196366423E-16));
#16466=CARTESIAN_POINT('Ctrl Pts',(-0.980948,-0.246942143572133,0.0201990724523192));
#16467=CARTESIAN_POINT('Ctrl Pts',(-0.980270995488453,-0.244251601209411,
0.0421062857595695));
#16468=CARTESIAN_POINT('Ctrl Pts',(-0.977553872336861,-0.232861760990032,
0.0842175114474169));
#16469=CARTESIAN_POINT('Ctrl Pts',(-0.975530745318961,-0.224161999508995,
0.104422493053066));
#16470=CARTESIAN_POINT('Ctrl Pts',(-0.971100730005489,-0.203463743702801,
0.139836317888042));
#16471=CARTESIAN_POINT('Ctrl Pts',(-0.968453058988463,-0.190326085855194,
0.15681442133453));
#16472=CARTESIAN_POINT('Ctrl Pts',(-0.963103647174702,-0.15976606450048,
0.1868781821531));
#16473=CARTESIAN_POINT('Ctrl Pts',(-0.960411259488514,-0.142345102874864,
0.199966927975188));
#16474=CARTESIAN_POINT('Ctrl Pts',(-0.955173119738174,-0.099930567888331,
0.223801617934945));
#16475=CARTESIAN_POINT('Ctrl Pts',(-0.952850216871763,-0.0740444353928835,
0.233157223576061));
#16476=CARTESIAN_POINT('Ctrl Pts',(-0.951592097314,-0.04763,0.238183666596899));
#16477=CARTESIAN_POINT('Origin',(0.,-0.04763,0.));
#16478=CARTESIAN_POINT('',(-0.841298510752802,-0.04763,-0.504455939115715));
#16479=CARTESIAN_POINT('Origin',(0.,-0.04763,0.));
#16480=CARTESIAN_POINT('Origin',(-0.707106781186547,-0.04763,-0.707106781186548));
#16481=CARTESIAN_POINT('Origin',(-0.707106781186547,0.,-0.707106781186548));
#16482=CARTESIAN_POINT('',(-0.504455939115715,-0.04763,-0.841298510752802));
#16483=CARTESIAN_POINT('Ctrl Pts',(-0.504455939115715,-0.04763,-0.841298510752802));
#16484=CARTESIAN_POINT('Ctrl Pts',(-0.508899795931835,-0.0740444353928835,
-0.838633903678357));
#16485=CARTESIAN_POINT('Ctrl Pts',(-0.517157748491652,-0.0999305678883309,
-0.833661031856294));
#16486=CARTESIAN_POINT('Ctrl Pts',(-0.537715343527944,-0.142345102874864,
-0.820511285096538));
#16487=CARTESIAN_POINT('Ctrl Pts',(-0.548874290046456,-0.159766064500479,
-0.813159949759));
#16488=CARTESIAN_POINT('Ctrl Pts',(-0.573915184558107,-0.190326085855194,
-0.795684265985089));
#16489=CARTESIAN_POINT('Ctrl Pts',(-0.587792702767295,-0.203463743702801,
-0.78555112003688));
#16490=CARTESIAN_POINT('Ctrl Pts',(-0.615966552324775,-0.224161999508995,
-0.763642258217233));
#16491=CARTESIAN_POINT('Ctrl Pts',(-0.631684198665438,-0.232861760990032,
-0.750785745543687));
#16492=CARTESIAN_POINT('Ctrl Pts',(-0.663382628119203,-0.244251601209411,
-0.722929908501543));
#16493=CARTESIAN_POINT('Ctrl Pts',(-0.679352081686668,-0.246942143572133,
-0.707917883896095));
#16494=CARTESIAN_POINT('Ctrl Pts',(-0.707917883896095,-0.246942143572133,
-0.679352081686668));
#16495=CARTESIAN_POINT('Ctrl Pts',(-0.722929908501543,-0.244251601209411,
-0.663382628119203));
#16496=CARTESIAN_POINT('Ctrl Pts',(-0.750785745543687,-0.232861760990032,
-0.631684198665439));
#16497=CARTESIAN_POINT('Ctrl Pts',(-0.763642258217232,-0.224161999508995,
-0.615966552324775));
#16498=CARTESIAN_POINT('Ctrl Pts',(-0.78555112003688,-0.203463743702801,
-0.587792702767295));
#16499=CARTESIAN_POINT('Ctrl Pts',(-0.795684265985088,-0.190326085855194,
-0.573915184558107));
#16500=CARTESIAN_POINT('Ctrl Pts',(-0.813159949759,-0.15976606450048,-0.548874290046456));
#16501=CARTESIAN_POINT('Ctrl Pts',(-0.820511285096538,-0.142345102874864,
-0.537715343527944));
#16502=CARTESIAN_POINT('Ctrl Pts',(-0.833661031856294,-0.0999305678883311,
-0.517157748491652));
#16503=CARTESIAN_POINT('Ctrl Pts',(-0.838633903678357,-0.0740444353928836,
-0.508899795931835));
#16504=CARTESIAN_POINT('Ctrl Pts',(-0.841298510752801,-0.04763,-0.504455939115715));
#16505=CARTESIAN_POINT('Origin',(-0.707106781186547,-0.04763,-0.707106781186548));
#16506=CARTESIAN_POINT('Origin',(0.,-0.04763,0.));
#16507=CARTESIAN_POINT('',(-0.238183666596899,-0.04763,-0.951592097314));
#16508=CARTESIAN_POINT('Origin',(0.,-0.04763,0.));
#16509=CARTESIAN_POINT('Origin',(5.55111512312578E-17,-0.04763,-1.));
#16510=CARTESIAN_POINT('Origin',(5.55111512312578E-17,0.,-1.));
#16511=CARTESIAN_POINT('',(0.238183666596899,-0.04763,-0.951592097314));
#16512=CARTESIAN_POINT('Ctrl Pts',(0.238183666596899,-0.04763,-0.951592097314));
#16513=CARTESIAN_POINT('Ctrl Pts',(0.233157223576062,-0.0740444353928835,
-0.952850216871763));
#16514=CARTESIAN_POINT('Ctrl Pts',(0.223801617934946,-0.099930567888331,
-0.955173119738174));
#16515=CARTESIAN_POINT('Ctrl Pts',(0.199966927975188,-0.142345102874864,
-0.960411259488514));
#16516=CARTESIAN_POINT('Ctrl Pts',(0.1868781821531,-0.15976606450048,-0.963103647174702));
#16517=CARTESIAN_POINT('Ctrl Pts',(0.15681442133453,-0.190326085855194,
-0.968453058988463));
#16518=CARTESIAN_POINT('Ctrl Pts',(0.139836317888042,-0.203463743702801,
-0.971100730005489));
#16519=CARTESIAN_POINT('Ctrl Pts',(0.104422493053067,-0.224161999508995,
-0.975530745318961));
#16520=CARTESIAN_POINT('Ctrl Pts',(0.0842175114474173,-0.232861760990032,
-0.977553872336861));
#16521=CARTESIAN_POINT('Ctrl Pts',(0.0421062857595698,-0.244251601209411,
-0.980270995488453));
#16522=CARTESIAN_POINT('Ctrl Pts',(0.0201990724523194,-0.246942143572133,
-0.980948));
#16523=CARTESIAN_POINT('Ctrl Pts',(-0.0201990724523193,-0.246942143572133,
-0.980948));
#16524=CARTESIAN_POINT('Ctrl Pts',(-0.0421062857595697,-0.244251601209411,
-0.980270995488453));
#16525=CARTESIAN_POINT('Ctrl Pts',(-0.0842175114474171,-0.232861760990032,
-0.977553872336861));
#16526=CARTESIAN_POINT('Ctrl Pts',(-0.104422493053067,-0.224161999508995,
-0.975530745318961));
#16527=CARTESIAN_POINT('Ctrl Pts',(-0.139836317888042,-0.203463743702801,
-0.971100730005489));
#16528=CARTESIAN_POINT('Ctrl Pts',(-0.15681442133453,-0.190326085855194,
-0.968453058988463));
#16529=CARTESIAN_POINT('Ctrl Pts',(-0.1868781821531,-0.15976606450048,-0.963103647174702));
#16530=CARTESIAN_POINT('Ctrl Pts',(-0.199966927975188,-0.142345102874864,
-0.960411259488514));
#16531=CARTESIAN_POINT('Ctrl Pts',(-0.223801617934945,-0.099930567888331,
-0.955173119738174));
#16532=CARTESIAN_POINT('Ctrl Pts',(-0.233157223576062,-0.0740444353928835,
-0.952850216871763));
#16533=CARTESIAN_POINT('Ctrl Pts',(-0.238183666596899,-0.0476299999999999,
-0.951592097314));
#16534=CARTESIAN_POINT('Origin',(5.55111512312578E-17,-0.04763,-1.));
#16535=CARTESIAN_POINT('Origin',(0.,-0.04763,0.));
#16536=CARTESIAN_POINT('',(0.504455939115715,-0.04763,-0.841298510752802));
#16537=CARTESIAN_POINT('Origin',(0.,-0.04763,0.));
#16538=CARTESIAN_POINT('Origin',(0.707106781186548,-0.04763,-0.707106781186547));
#16539=CARTESIAN_POINT('Origin',(0.707106781186548,0.,-0.707106781186547));
#16540=CARTESIAN_POINT('',(0.841298510752802,-0.04763,-0.504455939115715));
#16541=CARTESIAN_POINT('Ctrl Pts',(0.841298510752802,-0.04763,-0.504455939115715));
#16542=CARTESIAN_POINT('Ctrl Pts',(0.838633903678357,-0.0740444353928835,
-0.508899795931835));
#16543=CARTESIAN_POINT('Ctrl Pts',(0.833661031856294,-0.0999305678883309,
-0.517157748491652));
#16544=CARTESIAN_POINT('Ctrl Pts',(0.820511285096538,-0.142345102874864,
-0.537715343527944));
#16545=CARTESIAN_POINT('Ctrl Pts',(0.813159949759,-0.159766064500479,-0.548874290046456));
#16546=CARTESIAN_POINT('Ctrl Pts',(0.795684265985088,-0.190326085855194,
-0.573915184558107));
#16547=CARTESIAN_POINT('Ctrl Pts',(0.78555112003688,-0.203463743702801,
-0.587792702767295));
#16548=CARTESIAN_POINT('Ctrl Pts',(0.763642258217233,-0.224161999508995,
-0.615966552324775));
#16549=CARTESIAN_POINT('Ctrl Pts',(0.750785745543687,-0.232861760990032,
-0.631684198665438));
#16550=CARTESIAN_POINT('Ctrl Pts',(0.722929908501543,-0.244251601209411,
-0.663382628119203));
#16551=CARTESIAN_POINT('Ctrl Pts',(0.707917883896095,-0.246942143572133,
-0.679352081686668));
#16552=CARTESIAN_POINT('Ctrl Pts',(0.679352081686668,-0.246942143572133,
-0.707917883896095));
#16553=CARTESIAN_POINT('Ctrl Pts',(0.663382628119203,-0.244251601209411,
-0.722929908501543));
#16554=CARTESIAN_POINT('Ctrl Pts',(0.631684198665438,-0.232861760990032,
-0.750785745543687));
#16555=CARTESIAN_POINT('Ctrl Pts',(0.615966552324775,-0.224161999508995,
-0.763642258217232));
#16556=CARTESIAN_POINT('Ctrl Pts',(0.587792702767295,-0.203463743702801,
-0.78555112003688));
#16557=CARTESIAN_POINT('Ctrl Pts',(0.573915184558107,-0.190326085855194,
-0.795684265985088));
#16558=CARTESIAN_POINT('Ctrl Pts',(0.548874290046456,-0.159766064500479,
-0.813159949759));
#16559=CARTESIAN_POINT('Ctrl Pts',(0.537715343527944,-0.142345102874864,
-0.820511285096538));
#16560=CARTESIAN_POINT('Ctrl Pts',(0.517157748491652,-0.099930567888331,
-0.833661031856294));
#16561=CARTESIAN_POINT('Ctrl Pts',(0.508899795931835,-0.0740444353928835,
-0.838633903678357));
#16562=CARTESIAN_POINT('Ctrl Pts',(0.504455939115715,-0.04763,-0.841298510752801));
#16563=CARTESIAN_POINT('Origin',(0.707106781186548,-0.04763,-0.707106781186547));
#16564=CARTESIAN_POINT('Origin',(0.,-0.166705,0.));
#16565=CARTESIAN_POINT('',(-0.980948,-0.28578,1.20131482833E-16));
#16566=CARTESIAN_POINT('Origin',(0.,-0.28578,0.));
#16567=CARTESIAN_POINT('',(-0.980948,-0.166705,1.20131482833E-16));
#16568=CARTESIAN_POINT('',(0.951592097314,-0.04763,0.238183666596899));
#16569=CARTESIAN_POINT('Origin',(0.,-0.04763,0.));
#16570=CARTESIAN_POINT('',(0.951592097314,-0.04763,-0.238183666596899));
#16571=CARTESIAN_POINT('Ctrl Pts',(0.951592097314,-0.04763,0.238183666596899));
#16572=CARTESIAN_POINT('Ctrl Pts',(0.952850216871763,-0.0740444353928835,
0.233157223576062));
#16573=CARTESIAN_POINT('Ctrl Pts',(0.955173119738174,-0.099930567888331,
0.223801617934945));
#16574=CARTESIAN_POINT('Ctrl Pts',(0.960411259488514,-0.142345102874864,
0.199966927975188));
#16575=CARTESIAN_POINT('Ctrl Pts',(0.963103647174702,-0.15976606450048,
0.1868781821531));
#16576=CARTESIAN_POINT('Ctrl Pts',(0.968453058988463,-0.190326085855194,
0.15681442133453));
#16577=CARTESIAN_POINT('Ctrl Pts',(0.971100730005489,-0.203463743702801,
0.139836317888042));
#16578=CARTESIAN_POINT('Ctrl Pts',(0.975530745318961,-0.224161999508995,
0.104422493053067));
#16579=CARTESIAN_POINT('Ctrl Pts',(0.977553872336861,-0.232861760990032,
0.0842175114474172));
#16580=CARTESIAN_POINT('Ctrl Pts',(0.980270995488453,-0.244251601209411,
0.0421062857595697));
#16581=CARTESIAN_POINT('Ctrl Pts',(0.980948,-0.246942143572133,0.0201990724523194));
#16582=CARTESIAN_POINT('Ctrl Pts',(0.980948,-0.246942143572133,-0.0201990724523194));
#16583=CARTESIAN_POINT('Ctrl Pts',(0.980270995488453,-0.244251601209411,
-0.0421062857595697));
#16584=CARTESIAN_POINT('Ctrl Pts',(0.977553872336861,-0.232861760990032,
-0.0842175114474172));
#16585=CARTESIAN_POINT('Ctrl Pts',(0.975530745318961,-0.224161999508995,
-0.104422493053067));
#16586=CARTESIAN_POINT('Ctrl Pts',(0.971100730005489,-0.203463743702801,
-0.139836317888042));
#16587=CARTESIAN_POINT('Ctrl Pts',(0.968453058988463,-0.190326085855194,
-0.15681442133453));
#16588=CARTESIAN_POINT('Ctrl Pts',(0.963103647174702,-0.15976606450048,
-0.1868781821531));
#16589=CARTESIAN_POINT('Ctrl Pts',(0.960411259488514,-0.142345102874864,
-0.199966927975188));
#16590=CARTESIAN_POINT('Ctrl Pts',(0.955173119738174,-0.099930567888331,
-0.223801617934945));
#16591=CARTESIAN_POINT('Ctrl Pts',(0.952850216871763,-0.0740444353928835,
-0.233157223576062));
#16592=CARTESIAN_POINT('Ctrl Pts',(0.951592097314,-0.0476299999999999,-0.238183666596899));
#16593=CARTESIAN_POINT('Origin',(0.,-0.04763,0.));
#16594=CARTESIAN_POINT('Origin',(0.,-0.04763,0.));
#16595=CARTESIAN_POINT('Origin',(1.,-0.04763,0.));
#16596=CARTESIAN_POINT('Origin',(1.,0.,0.));
#16597=CARTESIAN_POINT('Origin',(1.,-0.04763,0.));
#16598=CARTESIAN_POINT('Origin',(0.,-0.28578,0.));
#16599=CARTESIAN_POINT('Origin',(0.,-0.04763,0.));
#16600=CARTESIAN_POINT('',(0.,0.,0.));
#16601=CARTESIAN_POINT('Origin',(1.013815,0.445,0.));
#16602=CARTESIAN_POINT('',(-1.013815,0.445,-1.24156529467757E-16));
#16603=CARTESIAN_POINT('Origin',(0.,0.445,0.));
#16604=CARTESIAN_POINT('',(-0.991185,0.445,-1.21385153761287E-16));
#16605=CARTESIAN_POINT('Origin',(0.,0.445,0.));
#16606=CARTESIAN_POINT('Origin',(0.,0.4075,0.));
#16607=CARTESIAN_POINT('',(-1.013815,0.37,-1.24156529467757E-16));
#16608=CARTESIAN_POINT('Origin',(0.,0.37,0.));
#16609=CARTESIAN_POINT('',(-1.013815,0.4075,-1.24156529467757E-16));
#16610=CARTESIAN_POINT('Origin',(0.991185,0.37,0.));
#16611=CARTESIAN_POINT('',(-0.991185,0.37,-1.21385153761287E-16));
#16612=CARTESIAN_POINT('Origin',(0.,0.37,0.));
#16613=CARTESIAN_POINT('Origin',(0.,0.4075,0.));
#16614=CARTESIAN_POINT('',(-0.991185,0.4075,-1.21385153761287E-16));
#16615=CARTESIAN_POINT('Origin',(1.013815,-0.37,0.));
#16616=CARTESIAN_POINT('',(-1.013815,-0.37,-1.24156529467757E-16));
#16617=CARTESIAN_POINT('Origin',(0.,-0.37,0.));
#16618=CARTESIAN_POINT('',(-0.991185,-0.37,-1.21385153761287E-16));
#16619=CARTESIAN_POINT('Origin',(0.,-0.37,0.));
#16620=CARTESIAN_POINT('Origin',(0.,-0.4075,0.));
#16621=CARTESIAN_POINT('',(-1.013815,-0.445,-1.24156529467757E-16));
#16622=CARTESIAN_POINT('Origin',(0.,-0.445,0.));
#16623=CARTESIAN_POINT('',(-1.013815,-0.4075,-1.24156529467757E-16));
#16624=CARTESIAN_POINT('Origin',(0.991185,-0.445,0.));
#16625=CARTESIAN_POINT('',(-0.991185,-0.445,-1.21385153761287E-16));
#16626=CARTESIAN_POINT('Origin',(0.,-0.445,0.));
#16627=CARTESIAN_POINT('Origin',(0.,-0.4075,0.));
#16628=CARTESIAN_POINT('',(-0.991185,-0.4075,-1.21385153761287E-16));
#16629=CARTESIAN_POINT('',(0.,0.,0.));
#16630=CARTESIAN_POINT('',(0.,0.,0.));
#16631=CARTESIAN_POINT('',(0.,0.,0.));
#16632=CARTESIAN_POINT('',(0.,0.,0.));
#16633=CARTESIAN_POINT('',(0.,0.,0.));
#16634=CARTESIAN_POINT('',(0.,0.,0.));
#16635=CARTESIAN_POINT('',(0.,0.,0.));
#16636=CARTESIAN_POINT('',(0.,0.,0.));
#16637=CARTESIAN_POINT('',(0.,0.,0.));
#16638=CARTESIAN_POINT('',(0.,0.,0.));
#16639=CARTESIAN_POINT('',(2.,2.95,10.));
#16640=CARTESIAN_POINT('',(12.,2.95,10.));
#16641=CARTESIAN_POINT('',(0.,0.,0.));
#16642=CARTESIAN_POINT('',(0.,0.,0.));
#16643=CARTESIAN_POINT('Origin',(12.,1.7,10.));
#16644=CARTESIAN_POINT('',(11.5,1.8,10.));
#16645=CARTESIAN_POINT('Origin',(12.,1.8,10.));
#16646=CARTESIAN_POINT('',(11.5,2.3,10.));
#16647=CARTESIAN_POINT('',(11.5,1.7,10.));
#16648=CARTESIAN_POINT('Origin',(12.,2.3,10.));
#16649=CARTESIAN_POINT('Origin',(12.,1.8,8.75));
#16650=CARTESIAN_POINT('',(13.,1.8,6.7));
#16651=CARTESIAN_POINT('',(11.,1.8,6.7));
#16652=CARTESIAN_POINT('',(12.,1.8,6.7));
#16653=CARTESIAN_POINT('',(13.,1.8,11.));
#16654=CARTESIAN_POINT('',(13.,1.8,6.5));
#16655=CARTESIAN_POINT('',(11.,1.8,11.));
#16656=CARTESIAN_POINT('',(13.,1.8,11.));
#16657=CARTESIAN_POINT('',(11.,1.8,11.));
#16658=CARTESIAN_POINT('Origin',(13.,1.8,11.));
#16659=CARTESIAN_POINT('',(13.,2.3,6.7));
#16660=CARTESIAN_POINT('',(13.,0.9,6.7));
#16661=CARTESIAN_POINT('',(13.,2.3,11.));
#16662=CARTESIAN_POINT('',(13.,2.3,6.5));
#16663=CARTESIAN_POINT('',(13.,1.8,11.));
#16664=CARTESIAN_POINT('Origin',(11.,1.8,6.5));
#16665=CARTESIAN_POINT('',(11.,2.3,6.7));
#16666=CARTESIAN_POINT('',(11.,0.9,6.7));
#16667=CARTESIAN_POINT('',(11.,2.3,11.));
#16668=CARTESIAN_POINT('',(11.,1.8,11.));
#16669=CARTESIAN_POINT('',(11.,2.3,11.));
#16670=CARTESIAN_POINT('Origin',(11.,1.8,11.));
#16671=CARTESIAN_POINT('',(13.,2.3,11.));
#16672=CARTESIAN_POINT('Origin',(12.,2.3,8.75));
#16673=CARTESIAN_POINT('',(12.,2.3,6.7));
#16674=CARTESIAN_POINT('Origin',(10.3,3.6,3.9));
#16675=CARTESIAN_POINT('',(10.4,3.6,4.065));
#16676=CARTESIAN_POINT('Origin',(10.4,3.6,3.9));
#16677=CARTESIAN_POINT('',(13.6,3.6,4.065));
#16678=CARTESIAN_POINT('',(10.3,3.6,4.065));
#16679=CARTESIAN_POINT('Origin',(13.6,3.6,3.9));
#16680=CARTESIAN_POINT('Origin',(10.3,-3.6,6.1));
#16681=CARTESIAN_POINT('',(10.4,-3.6,6.265));
#16682=CARTESIAN_POINT('Origin',(10.4,-3.6,6.1));
#16683=CARTESIAN_POINT('',(13.6,-3.6,6.265));
#16684=CARTESIAN_POINT('',(10.3,-3.6,6.265));
#16685=CARTESIAN_POINT('Origin',(13.6,-3.6,6.1));
#16686=CARTESIAN_POINT('Origin',(10.3,-3.6,3.9));
#16687=CARTESIAN_POINT('',(10.4,-3.6,4.065));
#16688=CARTESIAN_POINT('Origin',(10.4,-3.6,3.9));
#16689=CARTESIAN_POINT('',(13.6,-3.6,4.065));
#16690=CARTESIAN_POINT('',(10.3,-3.6,4.065));
#16691=CARTESIAN_POINT('Origin',(13.6,-3.6,3.9));
#16692=CARTESIAN_POINT('Origin',(10.3,3.6,6.1));
#16693=CARTESIAN_POINT('',(10.4,3.6,6.265));
#16694=CARTESIAN_POINT('Origin',(10.4,3.6,6.1));
#16695=CARTESIAN_POINT('',(13.6,3.6,6.265));
#16696=CARTESIAN_POINT('',(10.3,3.6,6.265));
#16697=CARTESIAN_POINT('Origin',(13.6,3.6,6.1));
#16698=CARTESIAN_POINT('Origin',(10.3,-2.5,5.));
#16699=CARTESIAN_POINT('',(10.4,-2.5,6.05));
#16700=CARTESIAN_POINT('Origin',(10.4,-2.5,5.));
#16701=CARTESIAN_POINT('',(13.6,-2.5,6.05));
#16702=CARTESIAN_POINT('',(10.3,-2.5,6.05));
#16703=CARTESIAN_POINT('Origin',(13.6,-2.5,5.));
#16704=CARTESIAN_POINT('Origin',(10.3,2.5,5.));
#16705=CARTESIAN_POINT('',(10.4,2.5,6.05));
#16706=CARTESIAN_POINT('Origin',(10.4,2.5,5.));
#16707=CARTESIAN_POINT('',(13.6,2.5,6.05));
#16708=CARTESIAN_POINT('',(10.3,2.5,6.05));
#16709=CARTESIAN_POINT('Origin',(13.6,2.5,5.));
#16710=CARTESIAN_POINT('Origin',(13.6,4.2,3.3));
#16711=CARTESIAN_POINT('',(13.6,4.2,3.3));
#16712=CARTESIAN_POINT('',(10.4,4.2,3.3));
#16713=CARTESIAN_POINT('',(13.6,4.2,3.3));
#16714=CARTESIAN_POINT('',(10.4,4.2,6.7));
#16715=CARTESIAN_POINT('',(10.4,4.2,3.3));
#16716=CARTESIAN_POINT('',(13.6,4.2,6.7));
#16717=CARTESIAN_POINT('',(13.6,4.2,6.7));
#16718=CARTESIAN_POINT('',(13.6,4.2,3.3));
#16719=CARTESIAN_POINT('Origin',(13.6,-4.2,3.3));
#16720=CARTESIAN_POINT('',(13.6,-4.2,3.3));
#16721=CARTESIAN_POINT('',(13.6,-4.2,3.3));
#16722=CARTESIAN_POINT('',(13.6,-4.2,6.7));
#16723=CARTESIAN_POINT('',(13.6,-4.2,6.7));
#16724=CARTESIAN_POINT('',(13.6,-4.2,3.3));
#16725=CARTESIAN_POINT('Origin',(10.4,-4.2,3.3));
#16726=CARTESIAN_POINT('',(10.4,-4.2,3.3));
#16727=CARTESIAN_POINT('',(10.4,-4.2,3.3));
#16728=CARTESIAN_POINT('',(10.4,-4.2,6.7));
#16729=CARTESIAN_POINT('',(10.4,-4.2,6.7));
#16730=CARTESIAN_POINT('',(10.4,-4.2,3.3));
#16731=CARTESIAN_POINT('Origin',(10.4,4.2,3.3));
#16732=CARTESIAN_POINT('',(10.4,4.2,3.3));
#16733=CARTESIAN_POINT('',(10.4,4.2,6.7));
#16734=CARTESIAN_POINT('Origin',(12.,0.,6.7));
#16735=CARTESIAN_POINT('Origin',(12.,0.,3.3));
#16736=CARTESIAN_POINT('',(0.,0.,0.));
#16737=CARTESIAN_POINT('Origin',(10.,3.6,3.9));
#16738=CARTESIAN_POINT('',(10.1,3.6,4.125));
#16739=CARTESIAN_POINT('Origin',(10.1,3.6,3.9));
#16740=CARTESIAN_POINT('',(10.4,3.6,4.125));
#16741=CARTESIAN_POINT('',(10.,3.6,4.125));
#16742=CARTESIAN_POINT('Origin',(10.4,3.6,3.9));
#16743=CARTESIAN_POINT('Origin',(10.,-3.6,6.1));
#16744=CARTESIAN_POINT('',(10.1,-3.6,6.325));
#16745=CARTESIAN_POINT('Origin',(10.1,-3.6,6.1));
#16746=CARTESIAN_POINT('',(10.4,-3.6,6.325));
#16747=CARTESIAN_POINT('',(10.,-3.6,6.325));
#16748=CARTESIAN_POINT('Origin',(10.4,-3.6,6.1));
#16749=CARTESIAN_POINT('Origin',(10.,-3.6,3.9));
#16750=CARTESIAN_POINT('',(10.1,-3.6,4.125));
#16751=CARTESIAN_POINT('Origin',(10.1,-3.6,3.9));
#16752=CARTESIAN_POINT('',(10.4,-3.6,4.125));
#16753=CARTESIAN_POINT('',(10.,-3.6,4.125));
#16754=CARTESIAN_POINT('Origin',(10.4,-3.6,3.9));
#16755=CARTESIAN_POINT('Origin',(10.,3.6,6.1));
#16756=CARTESIAN_POINT('',(10.1,3.6,6.325));
#16757=CARTESIAN_POINT('Origin',(10.1,3.6,6.1));
#16758=CARTESIAN_POINT('',(10.4,3.6,6.325));
#16759=CARTESIAN_POINT('',(10.,3.6,6.325));
#16760=CARTESIAN_POINT('Origin',(10.4,3.6,6.1));
#16761=CARTESIAN_POINT('Origin',(10.,-2.5,5.));
#16762=CARTESIAN_POINT('',(10.1,-2.5,5.7));
#16763=CARTESIAN_POINT('Origin',(10.1,-2.5,5.));
#16764=CARTESIAN_POINT('',(10.4,-2.5,5.7));
#16765=CARTESIAN_POINT('',(10.,-2.5,5.7));
#16766=CARTESIAN_POINT('Origin',(10.4,-2.5,5.));
#16767=CARTESIAN_POINT('Origin',(10.,2.5,5.));
#16768=CARTESIAN_POINT('',(10.1,2.5,5.7));
#16769=CARTESIAN_POINT('Origin',(10.1,2.5,5.));
#16770=CARTESIAN_POINT('',(10.4,2.5,5.7));
#16771=CARTESIAN_POINT('',(10.,2.5,5.7));
#16772=CARTESIAN_POINT('Origin',(10.4,2.5,5.));
#16773=CARTESIAN_POINT('Origin',(10.4,4.2,3.3));
#16774=CARTESIAN_POINT('',(10.4,4.2,3.3));
#16775=CARTESIAN_POINT('',(10.1,4.2,3.3));
#16776=CARTESIAN_POINT('',(10.4,4.2,3.3));
#16777=CARTESIAN_POINT('',(10.1,4.2,6.7));
#16778=CARTESIAN_POINT('',(10.1,4.2,3.3));
#16779=CARTESIAN_POINT('',(10.4,4.2,6.7));
#16780=CARTESIAN_POINT('',(10.4,4.2,6.7));
#16781=CARTESIAN_POINT('',(10.4,4.2,3.3));
#16782=CARTESIAN_POINT('Origin',(10.4,-4.2,3.3));
#16783=CARTESIAN_POINT('',(10.4,-4.2,3.3));
#16784=CARTESIAN_POINT('',(10.4,-4.2,3.3));
#16785=CARTESIAN_POINT('',(10.4,-4.2,6.7));
#16786=CARTESIAN_POINT('',(10.4,-4.2,6.7));
#16787=CARTESIAN_POINT('',(10.4,-4.2,3.3));
#16788=CARTESIAN_POINT('Origin',(10.1,-4.2,3.3));
#16789=CARTESIAN_POINT('',(10.1,-4.2,3.3));
#16790=CARTESIAN_POINT('',(10.1,-4.2,3.3));
#16791=CARTESIAN_POINT('',(10.1,-4.2,6.7));
#16792=CARTESIAN_POINT('',(10.1,-4.2,6.7));
#16793=CARTESIAN_POINT('',(10.1,-4.2,3.3));
#16794=CARTESIAN_POINT('Origin',(10.1,4.2,3.3));
#16795=CARTESIAN_POINT('',(10.1,4.2,3.3));
#16796=CARTESIAN_POINT('',(10.1,4.2,6.7));
#16797=CARTESIAN_POINT('Origin',(10.25,0.,6.7));
#16798=CARTESIAN_POINT('Origin',(10.25,0.,3.3));
#16799=CARTESIAN_POINT('',(0.,0.,0.));
#16800=CARTESIAN_POINT('Origin',(13.5,3.6,3.9));
#16801=CARTESIAN_POINT('',(13.6,3.6,4.125));
#16802=CARTESIAN_POINT('Origin',(13.6,3.6,3.9));
#16803=CARTESIAN_POINT('',(13.9,3.6,4.125));
#16804=CARTESIAN_POINT('',(13.5,3.6,4.125));
#16805=CARTESIAN_POINT('Origin',(13.9,3.6,3.9));
#16806=CARTESIAN_POINT('Origin',(13.5,-3.6,6.1));
#16807=CARTESIAN_POINT('',(13.6,-3.6,6.325));
#16808=CARTESIAN_POINT('Origin',(13.6,-3.6,6.1));
#16809=CARTESIAN_POINT('',(13.9,-3.6,6.325));
#16810=CARTESIAN_POINT('',(13.5,-3.6,6.325));
#16811=CARTESIAN_POINT('Origin',(13.9,-3.6,6.1));
#16812=CARTESIAN_POINT('Origin',(13.5,-3.6,3.9));
#16813=CARTESIAN_POINT('',(13.6,-3.6,4.125));
#16814=CARTESIAN_POINT('Origin',(13.6,-3.6,3.9));
#16815=CARTESIAN_POINT('',(13.9,-3.6,4.125));
#16816=CARTESIAN_POINT('',(13.5,-3.6,4.125));
#16817=CARTESIAN_POINT('Origin',(13.9,-3.6,3.9));
#16818=CARTESIAN_POINT('Origin',(13.5,3.6,6.1));
#16819=CARTESIAN_POINT('',(13.6,3.6,6.325));
#16820=CARTESIAN_POINT('Origin',(13.6,3.6,6.1));
#16821=CARTESIAN_POINT('',(13.9,3.6,6.325));
#16822=CARTESIAN_POINT('',(13.5,3.6,6.325));
#16823=CARTESIAN_POINT('Origin',(13.9,3.6,6.1));
#16824=CARTESIAN_POINT('Origin',(13.5,-2.5,5.));
#16825=CARTESIAN_POINT('',(13.6,-2.5,5.7));
#16826=CARTESIAN_POINT('Origin',(13.6,-2.5,5.));
#16827=CARTESIAN_POINT('',(13.9,-2.5,5.7));
#16828=CARTESIAN_POINT('',(13.5,-2.5,5.7));
#16829=CARTESIAN_POINT('Origin',(13.9,-2.5,5.));
#16830=CARTESIAN_POINT('Origin',(13.5,2.5,5.));
#16831=CARTESIAN_POINT('',(13.6,2.5,5.7));
#16832=CARTESIAN_POINT('Origin',(13.6,2.5,5.));
#16833=CARTESIAN_POINT('',(13.9,2.5,5.7));
#16834=CARTESIAN_POINT('',(13.5,2.5,5.7));
#16835=CARTESIAN_POINT('Origin',(13.9,2.5,5.));
#16836=CARTESIAN_POINT('Origin',(13.9,4.2,3.3));
#16837=CARTESIAN_POINT('',(13.9,4.2,3.3));
#16838=CARTESIAN_POINT('',(13.6,4.2,3.3));
#16839=CARTESIAN_POINT('',(13.9,4.2,3.3));
#16840=CARTESIAN_POINT('',(13.6,4.2,6.7));
#16841=CARTESIAN_POINT('',(13.6,4.2,3.3));
#16842=CARTESIAN_POINT('',(13.9,4.2,6.7));
#16843=CARTESIAN_POINT('',(13.9,4.2,6.7));
#16844=CARTESIAN_POINT('',(13.9,4.2,3.3));
#16845=CARTESIAN_POINT('Origin',(13.9,-4.2,3.3));
#16846=CARTESIAN_POINT('',(13.9,-4.2,3.3));
#16847=CARTESIAN_POINT('',(13.9,-4.2,3.3));
#16848=CARTESIAN_POINT('',(13.9,-4.2,6.7));
#16849=CARTESIAN_POINT('',(13.9,-4.2,6.7));
#16850=CARTESIAN_POINT('',(13.9,-4.2,3.3));
#16851=CARTESIAN_POINT('Origin',(13.6,-4.2,3.3));
#16852=CARTESIAN_POINT('',(13.6,-4.2,3.3));
#16853=CARTESIAN_POINT('',(13.6,-4.2,3.3));
#16854=CARTESIAN_POINT('',(13.6,-4.2,6.7));
#16855=CARTESIAN_POINT('',(13.6,-4.2,6.7));
#16856=CARTESIAN_POINT('',(13.6,-4.2,3.3));
#16857=CARTESIAN_POINT('Origin',(13.6,4.2,3.3));
#16858=CARTESIAN_POINT('',(13.6,4.2,3.3));
#16859=CARTESIAN_POINT('',(13.6,4.2,6.7));
#16860=CARTESIAN_POINT('Origin',(13.75,0.,6.7));
#16861=CARTESIAN_POINT('Origin',(13.75,0.,3.3));
#16862=CARTESIAN_POINT('',(0.,0.,0.));
#16863=CARTESIAN_POINT('Origin',(12.,2.7,10.));
#16864=CARTESIAN_POINT('',(11.835,2.7,10.));
#16865=CARTESIAN_POINT('Origin',(12.,2.7,10.));
#16866=CARTESIAN_POINT('',(11.835,3.8,10.));
#16867=CARTESIAN_POINT('',(11.835,2.7,10.));
#16868=CARTESIAN_POINT('Origin',(12.,3.8,10.));
#16869=CARTESIAN_POINT('Origin',(12.,2.7,10.));
#16870=CARTESIAN_POINT('Origin',(12.,1.8,10.));
#16871=CARTESIAN_POINT('',(11.2,1.8,10.));
#16872=CARTESIAN_POINT('Origin',(12.,1.8,10.));
#16873=CARTESIAN_POINT('',(11.5,1.8,10.));
#16874=CARTESIAN_POINT('Origin',(12.,1.8,10.));
#16875=CARTESIAN_POINT('Origin',(12.,1.4,10.));
#16876=CARTESIAN_POINT('',(11.2,1.4,10.));
#16877=CARTESIAN_POINT('',(11.2,1.4,10.));
#16878=CARTESIAN_POINT('Origin',(12.,1.4,10.));
#16879=CARTESIAN_POINT('Origin',(12.,1.4,10.));
#16880=CARTESIAN_POINT('Origin',(12.,1.8,10.));
#16881=CARTESIAN_POINT('',(11.5,3.8,10.));
#16882=CARTESIAN_POINT('Origin',(12.,3.8,10.));
#16883=CARTESIAN_POINT('',(11.5,1.8,10.));
#16884=CARTESIAN_POINT('Origin',(12.,3.8,10.));
#16885=CARTESIAN_POINT('',(0.,0.,0.));
#16886=CARTESIAN_POINT('Origin',(12.,2.3,10.));
#16887=CARTESIAN_POINT('',(11.495,2.5,10.));
#16888=CARTESIAN_POINT('Origin',(12.,2.5,10.));
#16889=CARTESIAN_POINT('',(11.495,2.3,10.));
#16890=CARTESIAN_POINT('',(11.495,2.3,10.));
#16891=CARTESIAN_POINT('Origin',(12.,2.3,10.));
#16892=CARTESIAN_POINT('Origin',(12.,2.3,10.));
#16893=CARTESIAN_POINT('',(11.3,2.5,10.));
#16894=CARTESIAN_POINT('Origin',(12.,2.5,10.));
#16895=CARTESIAN_POINT('',(11.3,2.3,10.));
#16896=CARTESIAN_POINT('',(11.3,2.3,10.));
#16897=CARTESIAN_POINT('Origin',(12.,2.3,10.));
#16898=CARTESIAN_POINT('Origin',(12.,2.5,10.));
#16899=CARTESIAN_POINT('Origin',(12.,2.3,10.));
#16900=CARTESIAN_POINT('',(0.,0.,0.));
#16901=CARTESIAN_POINT('Origin',(12.,3.4,10.));
#16902=CARTESIAN_POINT('',(11.495,3.8,10.));
#16903=CARTESIAN_POINT('Origin',(12.,3.8,10.));
#16904=CARTESIAN_POINT('',(11.495,3.4,10.));
#16905=CARTESIAN_POINT('',(11.495,3.4,10.));
#16906=CARTESIAN_POINT('Origin',(12.,3.4,10.));
#16907=CARTESIAN_POINT('Origin',(12.,3.4,10.));
#16908=CARTESIAN_POINT('',(11.3,3.8,10.));
#16909=CARTESIAN_POINT('Origin',(12.,3.8,10.));
#16910=CARTESIAN_POINT('',(11.3,3.4,10.));
#16911=CARTESIAN_POINT('',(11.3,3.4,10.));
#16912=CARTESIAN_POINT('Origin',(12.,3.4,10.));
#16913=CARTESIAN_POINT('Origin',(12.,3.8,10.));
#16914=CARTESIAN_POINT('Origin',(12.,3.4,10.));
#16915=CARTESIAN_POINT('',(0.,0.,0.));
#16916=CARTESIAN_POINT('Origin',(12.,3.8,10.));
#16917=CARTESIAN_POINT('',(11.775,4.,10.));
#16918=CARTESIAN_POINT('Origin',(12.,4.,10.));
#16919=CARTESIAN_POINT('',(11.775,3.8,10.));
#16920=CARTESIAN_POINT('',(11.775,3.8,10.));
#16921=CARTESIAN_POINT('Origin',(12.,3.8,10.));
#16922=CARTESIAN_POINT('Origin',(12.,3.8,10.));
#16923=CARTESIAN_POINT('',(11.2,4.,10.));
#16924=CARTESIAN_POINT('Origin',(12.,4.,10.));
#16925=CARTESIAN_POINT('',(11.2,3.8,10.));
#16926=CARTESIAN_POINT('',(11.2,3.8,10.));
#16927=CARTESIAN_POINT('Origin',(12.,3.8,10.));
#16928=CARTESIAN_POINT('Origin',(12.,4.,10.));
#16929=CARTESIAN_POINT('Origin',(12.,3.8,10.));
#16930=CARTESIAN_POINT('',(0.,0.,0.));
#16931=CARTESIAN_POINT('',(0.,0.,0.));
#16932=CARTESIAN_POINT('Origin',(0.75,1.2,0.));
#16933=CARTESIAN_POINT('',(0.885663593019381,1.2,-0.16));
#16934=CARTESIAN_POINT('',(0.885663593019381,1.2,0.16));
#16935=CARTESIAN_POINT('Origin',(0.,1.2,0.));
#16936=CARTESIAN_POINT('',(0.93,1.2,-0.16));
#16937=CARTESIAN_POINT('',(0.93,1.2,-0.16));
#16938=CARTESIAN_POINT('',(0.93,1.2,0.16));
#16939=CARTESIAN_POINT('',(0.93,1.2,0.16));
#16940=CARTESIAN_POINT('',(0.57,1.2,0.16));
#16941=CARTESIAN_POINT('Origin',(0.57,0.,0.16));
#16942=CARTESIAN_POINT('',(0.885663593019381,-1.2,0.16));
#16943=CARTESIAN_POINT('',(0.885663593019381,0.,0.16));
#16944=CARTESIAN_POINT('',(0.93,-1.2,0.16));
#16945=CARTESIAN_POINT('',(0.93,0.,0.16));
#16946=CARTESIAN_POINT('',(0.57,-1.2,0.16));
#16947=CARTESIAN_POINT('Origin',(0.75,-1.2,0.));
#16948=CARTESIAN_POINT('',(0.885663593019381,-1.2,-0.16));
#16949=CARTESIAN_POINT('Origin',(0.,-1.2,0.));
#16950=CARTESIAN_POINT('',(0.93,-1.2,-0.16));
#16951=CARTESIAN_POINT('',(0.93,-1.2,0.16));
#16952=CARTESIAN_POINT('',(0.93,-1.2,-0.16));
#16953=CARTESIAN_POINT('Origin',(0.93,0.,-0.16));
#16954=CARTESIAN_POINT('',(0.885663593019381,0.,-0.16));
#16955=CARTESIAN_POINT('',(0.93,0.,-0.16));
#16956=CARTESIAN_POINT('Origin',(0.93,0.,0.16));
#16957=CARTESIAN_POINT('Origin',(1.05,1.5,0.));
#16958=CARTESIAN_POINT('',(-1.05,1.5,-1.28587913910472E-16));
#16959=CARTESIAN_POINT('Origin',(0.,1.5,0.));
#16960=CARTESIAN_POINT('',(-0.9,1.5,-1.10218211923262E-16));
#16961=CARTESIAN_POINT('Origin',(0.,1.5,0.));
#16962=CARTESIAN_POINT('Origin',(0.,1.315,0.));
#16963=CARTESIAN_POINT('',(-1.05,1.13,-1.28587913910472E-16));
#16964=CARTESIAN_POINT('Origin',(0.,1.13,0.));
#16965=CARTESIAN_POINT('',(-1.05,1.315,-1.28587913910472E-16));
#16966=CARTESIAN_POINT('Origin',(1.,1.13,0.));
#16967=CARTESIAN_POINT('',(-1.,1.13,-1.22464679914735E-16));
#16968=CARTESIAN_POINT('Origin',(0.,1.13,0.));
#16969=CARTESIAN_POINT('Origin',(0.,1.065,0.));
#16970=CARTESIAN_POINT('',(-1.,1.,-1.22464679914735E-16));
#16971=CARTESIAN_POINT('Origin',(0.,1.,0.));
#16972=CARTESIAN_POINT('',(-1.,1.065,-1.22464679914735E-16));
#16973=CARTESIAN_POINT('Origin',(1.05,1.,0.));
#16974=CARTESIAN_POINT('',(-1.05,1.,-1.28587913910472E-16));
#16975=CARTESIAN_POINT('Origin',(0.,1.,0.));
#16976=CARTESIAN_POINT('Origin',(0.,0.,0.));
#16977=CARTESIAN_POINT('',(-1.05,-1.,-1.28587913910472E-16));
#16978=CARTESIAN_POINT('Origin',(0.,-1.,0.));
#16979=CARTESIAN_POINT('',(-1.05,0.,-1.28587913910472E-16));
#16980=CARTESIAN_POINT('Origin',(1.,-1.,0.));
#16981=CARTESIAN_POINT('',(-1.,-1.,-1.22464679914735E-16));
#16982=CARTESIAN_POINT('Origin',(0.,-1.,0.));
#16983=CARTESIAN_POINT('Origin',(0.,-1.065,0.));
#16984=CARTESIAN_POINT('',(-1.,-1.13,-1.22464679914735E-16));
#16985=CARTESIAN_POINT('Origin',(0.,-1.13,0.));
#16986=CARTESIAN_POINT('',(-1.,-1.065,-1.22464679914735E-16));
#16987=CARTESIAN_POINT('Origin',(1.05,-1.13,0.));
#16988=CARTESIAN_POINT('',(-1.05,-1.13,-1.28587913910472E-16));
#16989=CARTESIAN_POINT('Origin',(0.,-1.13,0.));
#16990=CARTESIAN_POINT('Origin',(0.,-1.315,0.));
#16991=CARTESIAN_POINT('',(-1.05,-1.5,-1.28587913910472E-16));
#16992=CARTESIAN_POINT('Origin',(0.,-1.5,0.));
#16993=CARTESIAN_POINT('',(-1.05,-1.315,-1.28587913910472E-16));
#16994=CARTESIAN_POINT('Origin',(0.9,-1.5,0.));
#16995=CARTESIAN_POINT('',(-0.9,-1.5,-1.10218211923262E-16));
#16996=CARTESIAN_POINT('Origin',(0.,-1.5,0.));
#16997=CARTESIAN_POINT('Origin',(0.,0.,0.));
#16998=CARTESIAN_POINT('',(-0.9,0.,-1.10218211923262E-16));
#16999=CARTESIAN_POINT('',(0.,0.,0.));
#17000=CARTESIAN_POINT('Origin',(0.75,1.2,0.));
#17001=CARTESIAN_POINT('',(0.880582193778639,1.2,0.16));
#17002=CARTESIAN_POINT('',(0.880582193778639,1.2,-0.16));
#17003=CARTESIAN_POINT('Origin',(0.,1.2,0.));
#17004=CARTESIAN_POINT('',(0.583459510163302,1.2,0.16));
#17005=CARTESIAN_POINT('',(0.57,1.2,0.16));
#17006=CARTESIAN_POINT('',(0.583459510163302,1.2,-0.16));
#17007=CARTESIAN_POINT('Origin',(0.,1.2,0.));
#17008=CARTESIAN_POINT('',(0.93,1.2,-0.16));
#17009=CARTESIAN_POINT('Origin',(0.93,0.,-0.16));
#17010=CARTESIAN_POINT('',(0.880582193778639,-1.2,-0.16));
#17011=CARTESIAN_POINT('',(0.880582193778639,0.,-0.16));
#17012=CARTESIAN_POINT('',(0.583459510163302,-1.2,-0.16));
#17013=CARTESIAN_POINT('',(0.583459510163302,0.,-0.16));
#17014=CARTESIAN_POINT('',(0.93,-1.2,-0.16));
#17015=CARTESIAN_POINT('Origin',(0.75,-1.2,0.));
#17016=CARTESIAN_POINT('',(0.880582193778639,-1.2,0.16));
#17017=CARTESIAN_POINT('Origin',(0.,-1.2,0.));
#17018=CARTESIAN_POINT('',(0.583459510163302,-1.2,0.16));
#17019=CARTESIAN_POINT('Origin',(0.,-1.2,0.));
#17020=CARTESIAN_POINT('',(0.57,-1.2,0.16));
#17021=CARTESIAN_POINT('Origin',(0.57,0.,0.16));
#17022=CARTESIAN_POINT('',(0.880582193778639,0.,0.16));
#17023=CARTESIAN_POINT('',(0.583459510163302,0.,0.16));
#17024=CARTESIAN_POINT('Origin',(0.895,1.35,0.));
#17025=CARTESIAN_POINT('',(-0.895,1.35,-1.09605888523688E-16));
#17026=CARTESIAN_POINT('Origin',(0.,1.35,0.));
#17027=CARTESIAN_POINT('',(-0.605,1.35,-7.40911313484149E-17));
#17028=CARTESIAN_POINT('Origin',(0.,1.35,0.));
#17029=CARTESIAN_POINT('Origin',(0.,0.,0.));
#17030=CARTESIAN_POINT('',(-0.895,-1.35,-1.09605888523688E-16));
#17031=CARTESIAN_POINT('Origin',(0.,-1.35,0.));
#17032=CARTESIAN_POINT('',(-0.895,0.,-1.09605888523688E-16));
#17033=CARTESIAN_POINT('Origin',(0.605,-1.35,0.));
#17034=CARTESIAN_POINT('',(-0.605,-1.35,-7.40911313484149E-17));
#17035=CARTESIAN_POINT('Origin',(0.,-1.35,0.));
#17036=CARTESIAN_POINT('Origin',(0.,0.,0.));
#17037=CARTESIAN_POINT('',(-0.605,0.,-7.40911313484149E-17));
#17038=CARTESIAN_POINT('',(0.,0.,0.));
#17039=CARTESIAN_POINT('',(0.,0.,0.));
#17040=CARTESIAN_POINT('',(0.,0.,0.));
#17041=CARTESIAN_POINT('Origin',(0.0866025403784439,-0.4,-0.15));
#17042=CARTESIAN_POINT('',(0.173205080756888,-0.4,0.));
#17043=CARTESIAN_POINT('',(0.0866025403784439,-0.4,-0.15));
#17044=CARTESIAN_POINT('',(0.173205080756888,-0.4,0.));
#17045=CARTESIAN_POINT('',(0.0866025403784439,-0.64,-0.15));
#17046=CARTESIAN_POINT('',(0.0866025403784439,-0.4,-0.15));
#17047=CARTESIAN_POINT('',(0.173205080756888,-0.64,0.));
#17048=CARTESIAN_POINT('',(0.173205080756888,-0.64,0.));
#17049=CARTESIAN_POINT('',(0.173205080756888,-0.4,0.));
#17050=CARTESIAN_POINT('Origin',(-0.0866025403784438,-0.4,-0.15));
#17051=CARTESIAN_POINT('',(-0.0866025403784438,-0.4,-0.15));
#17052=CARTESIAN_POINT('',(0.0866025403784439,-0.4,-0.15));
#17053=CARTESIAN_POINT('',(-0.0866025403784438,-0.64,-0.15));
#17054=CARTESIAN_POINT('',(-0.0866025403784438,-0.4,-0.15));
#17055=CARTESIAN_POINT('',(0.0866025403784439,-0.64,-0.15));
#17056=CARTESIAN_POINT('Origin',(-0.173205080756888,-0.4,-2.77555756156289E-17));
#17057=CARTESIAN_POINT('',(-0.173205080756888,-0.4,-2.12115047744981E-17));
#17058=CARTESIAN_POINT('',(-0.0866025403784438,-0.4,-0.15));
#17059=CARTESIAN_POINT('',(-0.173205080756888,-0.64,-2.77555756156289E-17));
#17060=CARTESIAN_POINT('',(-0.173205080756888,-0.4,-2.12115047744981E-17));
#17061=CARTESIAN_POINT('',(-0.0866025403784438,-0.64,-0.15));
#17062=CARTESIAN_POINT('Origin',(-0.0866025403784439,-0.4,0.15));
#17063=CARTESIAN_POINT('',(-0.0866025403784439,-0.4,0.15));
#17064=CARTESIAN_POINT('',(-0.173205080756888,-0.4,-2.12115047744981E-17));
#17065=CARTESIAN_POINT('',(-0.0866025403784439,-0.64,0.15));
#17066=CARTESIAN_POINT('',(-0.0866025403784439,-0.4,0.15));
#17067=CARTESIAN_POINT('',(-0.173205080756888,-0.64,-2.12115047744981E-17));
#17068=CARTESIAN_POINT('Origin',(0.0866025403784439,-0.4,0.15));
#17069=CARTESIAN_POINT('',(0.0866025403784439,-0.4,0.15));
#17070=CARTESIAN_POINT('',(-0.0866025403784439,-0.4,0.15));
#17071=CARTESIAN_POINT('',(0.0866025403784439,-0.64,0.15));
#17072=CARTESIAN_POINT('',(0.0866025403784439,-0.4,0.15));
#17073=CARTESIAN_POINT('',(-0.0866025403784439,-0.64,0.15));
#17074=CARTESIAN_POINT('Origin',(0.173205080756888,-0.4,0.));
#17075=CARTESIAN_POINT('',(0.0866025403784439,-0.4,0.15));
#17076=CARTESIAN_POINT('',(0.0866025403784439,-0.64,0.15));
#17077=CARTESIAN_POINT('Origin',(0.,-0.4,-2.77555756156289E-17));
#17078=CARTESIAN_POINT('Origin',(0.,-0.64,-2.77555756156289E-17));
#17079=CARTESIAN_POINT('Origin',(0.,-1.,0.));
#17080=CARTESIAN_POINT('',(-0.1954,-1.,2.39295984553393E-17));
#17081=CARTESIAN_POINT('Origin',(0.,-1.,0.));
#17082=CARTESIAN_POINT('Origin',(0.3,0.4,0.));
#17083=CARTESIAN_POINT('',(-0.3,0.4,-3.67394039744206E-17));
#17084=CARTESIAN_POINT('Origin',(0.,0.4,0.));
#17085=CARTESIAN_POINT('Origin',(0.,0.375,0.));
#17086=CARTESIAN_POINT('',(-0.35,0.35,-4.28626379701573E-17));
#17087=CARTESIAN_POINT('Origin',(0.,0.35,0.));
#17088=CARTESIAN_POINT('',(-0.325,0.375,-3.9801020972289E-17));
#17089=CARTESIAN_POINT('Origin',(0.,0.19,0.));
#17090=CARTESIAN_POINT('',(-0.35,0.03,-4.28626379701574E-17));
#17091=CARTESIAN_POINT('Origin',(0.,0.03,0.));
#17092=CARTESIAN_POINT('',(-0.35,0.19,-4.28626379701574E-17));
#17093=CARTESIAN_POINT('Origin',(0.,0.0149999999999999,0.));
#17094=CARTESIAN_POINT('',(-0.32,-3.29597460435593E-17,-3.91886975727153E-17));
#17095=CARTESIAN_POINT('Origin',(0.,0.,0.));
#17096=CARTESIAN_POINT('',(-0.335,0.0149999999999999,-4.10256677714363E-17));
#17097=CARTESIAN_POINT('Origin',(0.22,0.,0.));
#17098=CARTESIAN_POINT('',(-0.22,-6.93889390390723E-18,-2.69422295812418E-17));
#17099=CARTESIAN_POINT('Origin',(0.,0.,0.));
#17100=CARTESIAN_POINT('Origin',(0.,-0.02,0.));
#17101=CARTESIAN_POINT('',(-0.1954,-0.0492,2.39295984553393E-17));
#17102=CARTESIAN_POINT('Origin',(0.,-0.0492,0.));
#17103=CARTESIAN_POINT('',(-0.21,-0.02,-2.57175827820944E-17));
#17104=CARTESIAN_POINT('Origin',(0.,-0.8,0.));
#17105=CARTESIAN_POINT('',(-0.1954,-0.8,-2.39295984553393E-17));
#17106=CARTESIAN_POINT('',(0.,0.,0.));
#17107=CARTESIAN_POINT('',(0.,0.,0.));
#17108=CARTESIAN_POINT('',(0.,0.,0.));
#17109=CARTESIAN_POINT('',(0.,0.,0.));
#17110=CARTESIAN_POINT('',(0.,0.,0.));
#17111=CARTESIAN_POINT('',(0.,0.,0.));
#17112=CARTESIAN_POINT('',(0.,0.,0.));
#17113=CARTESIAN_POINT('',(0.,0.,0.));
#17114=CARTESIAN_POINT('',(0.,0.,0.));
#17115=CARTESIAN_POINT('',(0.,0.,0.));
#17116=CARTESIAN_POINT('',(0.,0.,0.));
#17117=CARTESIAN_POINT('',(-5.8,-16.5,2.2));
#17118=CARTESIAN_POINT('',(-5.8,-13.5,2.2));
#17119=CARTESIAN_POINT('',(5.8,-16.5,2.2));
#17120=CARTESIAN_POINT('',(5.8,-13.5,2.2));
#17121=CARTESIAN_POINT('',(0.,-15.,10.));
#17122=CARTESIAN_POINT('',(-4.75,-15.,7.87));
#17123=CARTESIAN_POINT('',(-4.75,-15.,8.03));
#17124=CARTESIAN_POINT('',(4.75,-15.,7.87));
#17125=CARTESIAN_POINT('',(4.75,-15.,8.03));
#17126=CARTESIAN_POINT('',(-5.8,-8.5,2.2));
#17127=CARTESIAN_POINT('',(-5.8,-5.5,2.2));
#17128=CARTESIAN_POINT('',(5.8,-8.5,2.2));
#17129=CARTESIAN_POINT('',(5.8,-5.5,2.2));
#17130=CARTESIAN_POINT('',(0.,-7.,10.));
#17131=CARTESIAN_POINT('',(-4.75,-7.,7.87));
#17132=CARTESIAN_POINT('',(-4.75,-7.,8.03));
#17133=CARTESIAN_POINT('',(4.75,-7.,7.87));
#17134=CARTESIAN_POINT('',(4.75,-7.,8.03));
#17135=CARTESIAN_POINT('',(4.,-2.5,2.7));
#17136=CARTESIAN_POINT('',(4.,-4.1,3.3));
#17137=CARTESIAN_POINT('',(4.,-4.1,3.4));
#17138=CARTESIAN_POINT('',(4.,-0.9,3.3));
#17139=CARTESIAN_POINT('',(4.,-0.9,3.4));
#17140=CARTESIAN_POINT('',(4.,-3.7,6.05));
#17141=CARTESIAN_POINT('',(4.,2.5,2.7));
#17142=CARTESIAN_POINT('',(4.,0.9,3.3));
#17143=CARTESIAN_POINT('',(4.,0.9,3.4));
#17144=CARTESIAN_POINT('',(4.,4.1,3.3));
#17145=CARTESIAN_POINT('',(4.,4.1,3.4));
#17146=CARTESIAN_POINT('',(4.,1.3,6.05));
#17147=CARTESIAN_POINT('',(3.2,0.,1.6));
#17148=CARTESIAN_POINT('',(4.8,0.,1.6));
#17149=CARTESIAN_POINT('',(20.,-2.5,2.7));
#17150=CARTESIAN_POINT('',(20.,-4.1,3.3));
#17151=CARTESIAN_POINT('',(20.,-4.1,3.4));
#17152=CARTESIAN_POINT('',(20.,-0.9,3.3));
#17153=CARTESIAN_POINT('',(20.,-0.9,3.4));
#17154=CARTESIAN_POINT('',(20.,-3.7,6.05));
#17155=CARTESIAN_POINT('',(20.,2.5,2.7));
#17156=CARTESIAN_POINT('',(20.,0.9,3.3));
#17157=CARTESIAN_POINT('',(20.,0.9,3.4));
#17158=CARTESIAN_POINT('',(20.,4.1,3.3));
#17159=CARTESIAN_POINT('',(20.,4.1,3.4));
#17160=CARTESIAN_POINT('',(20.,1.3,6.05));
#17161=CARTESIAN_POINT('',(19.2,0.,1.6));
#17162=CARTESIAN_POINT('',(20.8,0.,1.6));
#17163=CARTESIAN_POINT('',(2.,-2.5,5.));
#17164=CARTESIAN_POINT('',(2.,2.5,5.));
#17165=CARTESIAN_POINT('',(0.,0.,0.));
#17166=CARTESIAN_POINT('',(0.,0.,0.));
#17167=CARTESIAN_POINT('',(0.,0.,0.));
#17168=CARTESIAN_POINT('',(0.,0.,0.));
#17169=CARTESIAN_POINT('',(0.,0.,0.));
#17170=CARTESIAN_POINT('',(0.,0.,0.));
#17171=CARTESIAN_POINT('',(0.,0.,0.));
#17172=CARTESIAN_POINT('',(0.,0.,0.));
#17173=CARTESIAN_POINT('',(0.,0.,0.));
#17174=CARTESIAN_POINT('',(0.,0.,9.35));
#17175=CARTESIAN_POINT('',(0.,-17.05,11.8));
#17176=CARTESIAN_POINT('',(0.,-4.15,11.8));
#17177=CARTESIAN_POINT('',(0.,-1.3,11.8));
#17178=CARTESIAN_POINT('',(2.,4.,10.));
#17179=CARTESIAN_POINT('',(0.,0.,0.));
#17180=CARTESIAN_POINT('',(0.,0.,0.));
#17181=CARTESIAN_POINT('',(0.,0.,0.));
#17182=CARTESIAN_POINT('',(0.,0.,0.));
#17183=CARTESIAN_POINT('',(0.,0.,0.));
#17184=CARTESIAN_POINT('',(0.,0.,0.));
#17185=CARTESIAN_POINT('',(0.,0.,0.));
#17186=CARTESIAN_POINT('',(12.,-2.5,5.));
#17187=CARTESIAN_POINT('',(12.,2.5,5.));
#17188=CARTESIAN_POINT('',(10.1,-3.6,3.9));
#17189=CARTESIAN_POINT('',(10.1,-3.6,6.1));
#17190=CARTESIAN_POINT('',(10.1,3.6,3.9));
#17191=CARTESIAN_POINT('',(10.1,3.6,6.1));
#17192=CARTESIAN_POINT('',(13.9,-3.6,3.9));
#17193=CARTESIAN_POINT('',(13.9,-3.6,6.1));
#17194=CARTESIAN_POINT('',(13.9,3.6,3.9));
#17195=CARTESIAN_POINT('',(13.9,3.6,6.1));
#17196=CARTESIAN_POINT('',(12.,4.,10.));
#17197=CARTESIAN_POINT('',(0.,0.,0.));
#17198=CARTESIAN_POINT('',(0.,0.,0.));
#17199=CARTESIAN_POINT('',(0.,0.,0.));
#17200=CARTESIAN_POINT('',(0.,0.,0.));
#17201=UNCERTAINTY_MEASURE_WITH_UNIT(LENGTH_MEASURE(0.001),#17323,
'DISTANCE_ACCURACY_VALUE',
'Maximum model space distance between geometric entities at asserted c
onnectivities');
#17202=UNCERTAINTY_MEASURE_WITH_UNIT(LENGTH_MEASURE(0.001),#17323,
'DISTANCE_ACCURACY_VALUE',
'Maximum model space distance between geometric entities at asserted c
onnectivities');
#17203=UNCERTAINTY_MEASURE_WITH_UNIT(LENGTH_MEASURE(0.001),#17323,
'DISTANCE_ACCURACY_VALUE',
'Maximum model space distance between geometric entities at asserted c
onnectivities');
#17204=UNCERTAINTY_MEASURE_WITH_UNIT(LENGTH_MEASURE(0.001),#17323,
'DISTANCE_ACCURACY_VALUE',
'Maximum model space distance between geometric entities at asserted c
onnectivities');
#17205=UNCERTAINTY_MEASURE_WITH_UNIT(LENGTH_MEASURE(0.001),#17323,
'DISTANCE_ACCURACY_VALUE',
'Maximum model space distance between geometric entities at asserted c
onnectivities');
#17206=UNCERTAINTY_MEASURE_WITH_UNIT(LENGTH_MEASURE(0.001),#17323,
'DISTANCE_ACCURACY_VALUE',
'Maximum model space distance between geometric entities at asserted c
onnectivities');
#17207=UNCERTAINTY_MEASURE_WITH_UNIT(LENGTH_MEASURE(0.001),#17323,
'DISTANCE_ACCURACY_VALUE',
'Maximum model space distance between geometric entities at asserted c
onnectivities');
#17208=UNCERTAINTY_MEASURE_WITH_UNIT(LENGTH_MEASURE(0.001),#17323,
'DISTANCE_ACCURACY_VALUE',
'Maximum model space distance between geometric entities at asserted c
onnectivities');
#17209=UNCERTAINTY_MEASURE_WITH_UNIT(LENGTH_MEASURE(0.001),#17323,
'DISTANCE_ACCURACY_VALUE',
'Maximum model space distance between geometric entities at asserted c
onnectivities');
#17210=UNCERTAINTY_MEASURE_WITH_UNIT(LENGTH_MEASURE(0.001),#17323,
'DISTANCE_ACCURACY_VALUE',
'Maximum model space distance between geometric entities at asserted c
onnectivities');
#17211=UNCERTAINTY_MEASURE_WITH_UNIT(LENGTH_MEASURE(0.001),#17323,
'DISTANCE_ACCURACY_VALUE',
'Maximum model space distance between geometric entities at asserted c
onnectivities');
#17212=UNCERTAINTY_MEASURE_WITH_UNIT(LENGTH_MEASURE(0.001),#17323,
'DISTANCE_ACCURACY_VALUE',
'Maximum model space distance between geometric entities at asserted c
onnectivities');
#17213=UNCERTAINTY_MEASURE_WITH_UNIT(LENGTH_MEASURE(0.001),#17323,
'DISTANCE_ACCURACY_VALUE',
'Maximum model space distance between geometric entities at asserted c
onnectivities');
#17214=UNCERTAINTY_MEASURE_WITH_UNIT(LENGTH_MEASURE(0.001),#17323,
'DISTANCE_ACCURACY_VALUE',
'Maximum model space distance between geometric entities at asserted c
onnectivities');
#17215=UNCERTAINTY_MEASURE_WITH_UNIT(LENGTH_MEASURE(0.001),#17323,
'DISTANCE_ACCURACY_VALUE',
'Maximum model space distance between geometric entities at asserted c
onnectivities');
#17216=UNCERTAINTY_MEASURE_WITH_UNIT(LENGTH_MEASURE(0.001),#17323,
'DISTANCE_ACCURACY_VALUE',
'Maximum model space distance between geometric entities at asserted c
onnectivities');
#17217=UNCERTAINTY_MEASURE_WITH_UNIT(LENGTH_MEASURE(0.001),#17323,
'DISTANCE_ACCURACY_VALUE',
'Maximum model space distance between geometric entities at asserted c
onnectivities');
#17218=UNCERTAINTY_MEASURE_WITH_UNIT(LENGTH_MEASURE(0.001),#17323,
'DISTANCE_ACCURACY_VALUE',
'Maximum model space distance between geometric entities at asserted c
onnectivities');
#17219=UNCERTAINTY_MEASURE_WITH_UNIT(LENGTH_MEASURE(0.001),#17323,
'DISTANCE_ACCURACY_VALUE',
'Maximum model space distance between geometric entities at asserted c
onnectivities');
#17220=UNCERTAINTY_MEASURE_WITH_UNIT(LENGTH_MEASURE(0.001),#17323,
'DISTANCE_ACCURACY_VALUE',
'Maximum model space distance between geometric entities at asserted c
onnectivities');
#17221=UNCERTAINTY_MEASURE_WITH_UNIT(LENGTH_MEASURE(0.001),#17323,
'DISTANCE_ACCURACY_VALUE',
'Maximum model space distance between geometric entities at asserted c
onnectivities');
#17222=UNCERTAINTY_MEASURE_WITH_UNIT(LENGTH_MEASURE(0.001),#17323,
'DISTANCE_ACCURACY_VALUE',
'Maximum model space distance between geometric entities at asserted c
onnectivities');
#17223=UNCERTAINTY_MEASURE_WITH_UNIT(LENGTH_MEASURE(0.001),#17323,
'DISTANCE_ACCURACY_VALUE',
'Maximum model space distance between geometric entities at asserted c
onnectivities');
#17224=UNCERTAINTY_MEASURE_WITH_UNIT(LENGTH_MEASURE(0.001),#17323,
'DISTANCE_ACCURACY_VALUE',
'Maximum model space distance between geometric entities at asserted c
onnectivities');
#17225=UNCERTAINTY_MEASURE_WITH_UNIT(LENGTH_MEASURE(0.001),#17323,
'DISTANCE_ACCURACY_VALUE',
'Maximum model space distance between geometric entities at asserted c
onnectivities');
#17226=UNCERTAINTY_MEASURE_WITH_UNIT(LENGTH_MEASURE(0.001),#17323,
'DISTANCE_ACCURACY_VALUE',
'Maximum model space distance between geometric entities at asserted c
onnectivities');
#17227=UNCERTAINTY_MEASURE_WITH_UNIT(LENGTH_MEASURE(0.001),#17323,
'DISTANCE_ACCURACY_VALUE',
'Maximum model space distance between geometric entities at asserted c
onnectivities');
#17228=UNCERTAINTY_MEASURE_WITH_UNIT(LENGTH_MEASURE(0.001),#17323,
'DISTANCE_ACCURACY_VALUE',
'Maximum model space distance between geometric entities at asserted c
onnectivities');
#17229=UNCERTAINTY_MEASURE_WITH_UNIT(LENGTH_MEASURE(0.001),#17323,
'DISTANCE_ACCURACY_VALUE',
'Maximum model space distance between geometric entities at asserted c
onnectivities');
#17230=UNCERTAINTY_MEASURE_WITH_UNIT(LENGTH_MEASURE(0.001),#17323,
'DISTANCE_ACCURACY_VALUE',
'Maximum model space distance between geometric entities at asserted c
onnectivities');
#17231=UNCERTAINTY_MEASURE_WITH_UNIT(LENGTH_MEASURE(0.001),#17323,
'DISTANCE_ACCURACY_VALUE',
'Maximum model space distance between geometric entities at asserted c
onnectivities');
#17232=UNCERTAINTY_MEASURE_WITH_UNIT(LENGTH_MEASURE(0.001),#17323,
'DISTANCE_ACCURACY_VALUE',
'Maximum model space distance between geometric entities at asserted c
onnectivities');
#17233=UNCERTAINTY_MEASURE_WITH_UNIT(LENGTH_MEASURE(0.001),#17323,
'DISTANCE_ACCURACY_VALUE',
'Maximum model space distance between geometric entities at asserted c
onnectivities');
#17234=UNCERTAINTY_MEASURE_WITH_UNIT(LENGTH_MEASURE(0.001),#17323,
'DISTANCE_ACCURACY_VALUE',
'Maximum model space distance between geometric entities at asserted c
onnectivities');
#17235=UNCERTAINTY_MEASURE_WITH_UNIT(LENGTH_MEASURE(0.001),#17323,
'DISTANCE_ACCURACY_VALUE',
'Maximum model space distance between geometric entities at asserted c
onnectivities');
#17236=UNCERTAINTY_MEASURE_WITH_UNIT(LENGTH_MEASURE(0.001),#17323,
'DISTANCE_ACCURACY_VALUE',
'Maximum model space distance between geometric entities at asserted c
onnectivities');
#17237=UNCERTAINTY_MEASURE_WITH_UNIT(LENGTH_MEASURE(0.001),#17323,
'DISTANCE_ACCURACY_VALUE',
'Maximum model space distance between geometric entities at asserted c
onnectivities');
#17238=UNCERTAINTY_MEASURE_WITH_UNIT(LENGTH_MEASURE(0.001),#17323,
'DISTANCE_ACCURACY_VALUE',
'Maximum model space distance between geometric entities at asserted c
onnectivities');
#17239=UNCERTAINTY_MEASURE_WITH_UNIT(LENGTH_MEASURE(0.001),#17323,
'DISTANCE_ACCURACY_VALUE',
'Maximum model space distance between geometric entities at asserted c
onnectivities');
#17240=UNCERTAINTY_MEASURE_WITH_UNIT(LENGTH_MEASURE(0.001),#17323,
'DISTANCE_ACCURACY_VALUE',
'Maximum model space distance between geometric entities at asserted c
onnectivities');
#17241=UNCERTAINTY_MEASURE_WITH_UNIT(LENGTH_MEASURE(0.001),#17323,
'DISTANCE_ACCURACY_VALUE',
'Maximum model space distance between geometric entities at asserted c
onnectivities');
#17242=UNCERTAINTY_MEASURE_WITH_UNIT(LENGTH_MEASURE(0.001),#17323,
'DISTANCE_ACCURACY_VALUE',
'Maximum model space distance between geometric entities at asserted c
onnectivities');
#17243=UNCERTAINTY_MEASURE_WITH_UNIT(LENGTH_MEASURE(0.001),#17323,
'DISTANCE_ACCURACY_VALUE',
'Maximum model space distance between geometric entities at asserted c
onnectivities');
#17244=UNCERTAINTY_MEASURE_WITH_UNIT(LENGTH_MEASURE(0.001),#17323,
'DISTANCE_ACCURACY_VALUE',
'Maximum model space distance between geometric entities at asserted c
onnectivities');
#17245=UNCERTAINTY_MEASURE_WITH_UNIT(LENGTH_MEASURE(0.001),#17323,
'DISTANCE_ACCURACY_VALUE',
'Maximum model space distance between geometric entities at asserted c
onnectivities');
#17246=UNCERTAINTY_MEASURE_WITH_UNIT(LENGTH_MEASURE(0.001),#17323,
'DISTANCE_ACCURACY_VALUE',
'Maximum model space distance between geometric entities at asserted c
onnectivities');
#17247=UNCERTAINTY_MEASURE_WITH_UNIT(LENGTH_MEASURE(0.001),#17323,
'DISTANCE_ACCURACY_VALUE',
'Maximum model space distance between geometric entities at asserted c
onnectivities');
#17248=UNCERTAINTY_MEASURE_WITH_UNIT(LENGTH_MEASURE(0.001),#17323,
'DISTANCE_ACCURACY_VALUE',
'Maximum model space distance between geometric entities at asserted c
onnectivities');
#17249=UNCERTAINTY_MEASURE_WITH_UNIT(LENGTH_MEASURE(0.001),#17323,
'DISTANCE_ACCURACY_VALUE',
'Maximum model space distance between geometric entities at asserted c
onnectivities');
#17250=UNCERTAINTY_MEASURE_WITH_UNIT(LENGTH_MEASURE(0.001),#17323,
'DISTANCE_ACCURACY_VALUE',
'Maximum model space distance between geometric entities at asserted c
onnectivities');
#17251=UNCERTAINTY_MEASURE_WITH_UNIT(LENGTH_MEASURE(0.001),#17323,
'DISTANCE_ACCURACY_VALUE',
'Maximum model space distance between geometric entities at asserted c
onnectivities');
#17252=UNCERTAINTY_MEASURE_WITH_UNIT(LENGTH_MEASURE(0.001),#17323,
'DISTANCE_ACCURACY_VALUE',
'Maximum model space distance between geometric entities at asserted c
onnectivities');
#17253=UNCERTAINTY_MEASURE_WITH_UNIT(LENGTH_MEASURE(0.001),#17323,
'DISTANCE_ACCURACY_VALUE',
'Maximum model space distance between geometric entities at asserted c
onnectivities');
#17254=UNCERTAINTY_MEASURE_WITH_UNIT(LENGTH_MEASURE(0.001),#17323,
'DISTANCE_ACCURACY_VALUE',
'Maximum model space distance between geometric entities at asserted c
onnectivities');
#17255=UNCERTAINTY_MEASURE_WITH_UNIT(LENGTH_MEASURE(0.001),#17323,
'DISTANCE_ACCURACY_VALUE',
'Maximum model space distance between geometric entities at asserted c
onnectivities');
#17256=UNCERTAINTY_MEASURE_WITH_UNIT(LENGTH_MEASURE(0.001),#17323,
'DISTANCE_ACCURACY_VALUE',
'Maximum model space distance between geometric entities at asserted c
onnectivities');
#17257=UNCERTAINTY_MEASURE_WITH_UNIT(LENGTH_MEASURE(0.001),#17323,
'DISTANCE_ACCURACY_VALUE',
'Maximum model space distance between geometric entities at asserted c
onnectivities');
#17258=UNCERTAINTY_MEASURE_WITH_UNIT(LENGTH_MEASURE(0.001),#17323,
'DISTANCE_ACCURACY_VALUE',
'Maximum model space distance between geometric entities at asserted c
onnectivities');
#17259=UNCERTAINTY_MEASURE_WITH_UNIT(LENGTH_MEASURE(0.001),#17323,
'DISTANCE_ACCURACY_VALUE',
'Maximum model space distance between geometric entities at asserted c
onnectivities');
#17260=UNCERTAINTY_MEASURE_WITH_UNIT(LENGTH_MEASURE(0.001),#17323,
'DISTANCE_ACCURACY_VALUE',
'Maximum model space distance between geometric entities at asserted c
onnectivities');
#17261=UNCERTAINTY_MEASURE_WITH_UNIT(LENGTH_MEASURE(0.001),#17323,
'DISTANCE_ACCURACY_VALUE',
'Maximum model space distance between geometric entities at asserted c
onnectivities');
#17262=(
GEOMETRIC_REPRESENTATION_CONTEXT(3)
GLOBAL_UNCERTAINTY_ASSIGNED_CONTEXT((#17201))
GLOBAL_UNIT_ASSIGNED_CONTEXT((#17323,#17325,#17326))
REPRESENTATION_CONTEXT('','3D')
);
#17263=(
GEOMETRIC_REPRESENTATION_CONTEXT(3)
GLOBAL_UNCERTAINTY_ASSIGNED_CONTEXT((#17202))
GLOBAL_UNIT_ASSIGNED_CONTEXT((#17323,#17325,#17326))
REPRESENTATION_CONTEXT('','3D')
);
#17264=(
GEOMETRIC_REPRESENTATION_CONTEXT(3)
GLOBAL_UNCERTAINTY_ASSIGNED_CONTEXT((#17203))
GLOBAL_UNIT_ASSIGNED_CONTEXT((#17323,#17325,#17326))
REPRESENTATION_CONTEXT('','3D')
);
#17265=(
GEOMETRIC_REPRESENTATION_CONTEXT(3)
GLOBAL_UNCERTAINTY_ASSIGNED_CONTEXT((#17204))
GLOBAL_UNIT_ASSIGNED_CONTEXT((#17323,#17325,#17326))
REPRESENTATION_CONTEXT('','3D')
);
#17266=(
GEOMETRIC_REPRESENTATION_CONTEXT(3)
GLOBAL_UNCERTAINTY_ASSIGNED_CONTEXT((#17205))
GLOBAL_UNIT_ASSIGNED_CONTEXT((#17323,#17325,#17326))
REPRESENTATION_CONTEXT('','3D')
);
#17267=(
GEOMETRIC_REPRESENTATION_CONTEXT(3)
GLOBAL_UNCERTAINTY_ASSIGNED_CONTEXT((#17206))
GLOBAL_UNIT_ASSIGNED_CONTEXT((#17323,#17325,#17326))
REPRESENTATION_CONTEXT('','3D')
);
#17268=(
GEOMETRIC_REPRESENTATION_CONTEXT(3)
GLOBAL_UNCERTAINTY_ASSIGNED_CONTEXT((#17207))
GLOBAL_UNIT_ASSIGNED_CONTEXT((#17323,#17325,#17326))
REPRESENTATION_CONTEXT('','3D')
);
#17269=(
GEOMETRIC_REPRESENTATION_CONTEXT(3)
GLOBAL_UNCERTAINTY_ASSIGNED_CONTEXT((#17208))
GLOBAL_UNIT_ASSIGNED_CONTEXT((#17323,#17325,#17326))
REPRESENTATION_CONTEXT('','3D')
);
#17270=(
GEOMETRIC_REPRESENTATION_CONTEXT(3)
GLOBAL_UNCERTAINTY_ASSIGNED_CONTEXT((#17209))
GLOBAL_UNIT_ASSIGNED_CONTEXT((#17323,#17325,#17326))
REPRESENTATION_CONTEXT('','3D')
);
#17271=(
GEOMETRIC_REPRESENTATION_CONTEXT(3)
GLOBAL_UNCERTAINTY_ASSIGNED_CONTEXT((#17210))
GLOBAL_UNIT_ASSIGNED_CONTEXT((#17323,#17325,#17326))
REPRESENTATION_CONTEXT('','3D')
);
#17272=(
GEOMETRIC_REPRESENTATION_CONTEXT(3)
GLOBAL_UNCERTAINTY_ASSIGNED_CONTEXT((#17211))
GLOBAL_UNIT_ASSIGNED_CONTEXT((#17323,#17325,#17326))
REPRESENTATION_CONTEXT('','3D')
);
#17273=(
GEOMETRIC_REPRESENTATION_CONTEXT(3)
GLOBAL_UNCERTAINTY_ASSIGNED_CONTEXT((#17212))
GLOBAL_UNIT_ASSIGNED_CONTEXT((#17323,#17325,#17326))
REPRESENTATION_CONTEXT('','3D')
);
#17274=(
GEOMETRIC_REPRESENTATION_CONTEXT(3)
GLOBAL_UNCERTAINTY_ASSIGNED_CONTEXT((#17213))
GLOBAL_UNIT_ASSIGNED_CONTEXT((#17323,#17325,#17326))
REPRESENTATION_CONTEXT('','3D')
);
#17275=(
GEOMETRIC_REPRESENTATION_CONTEXT(3)
GLOBAL_UNCERTAINTY_ASSIGNED_CONTEXT((#17214))
GLOBAL_UNIT_ASSIGNED_CONTEXT((#17323,#17325,#17326))
REPRESENTATION_CONTEXT('','3D')
);
#17276=(
GEOMETRIC_REPRESENTATION_CONTEXT(3)
GLOBAL_UNCERTAINTY_ASSIGNED_CONTEXT((#17215))
GLOBAL_UNIT_ASSIGNED_CONTEXT((#17323,#17325,#17326))
REPRESENTATION_CONTEXT('','3D')
);
#17277=(
GEOMETRIC_REPRESENTATION_CONTEXT(3)
GLOBAL_UNCERTAINTY_ASSIGNED_CONTEXT((#17216))
GLOBAL_UNIT_ASSIGNED_CONTEXT((#17323,#17325,#17326))
REPRESENTATION_CONTEXT('','3D')
);
#17278=(
GEOMETRIC_REPRESENTATION_CONTEXT(3)
GLOBAL_UNCERTAINTY_ASSIGNED_CONTEXT((#17217))
GLOBAL_UNIT_ASSIGNED_CONTEXT((#17323,#17325,#17326))
REPRESENTATION_CONTEXT('','3D')
);
#17279=(
GEOMETRIC_REPRESENTATION_CONTEXT(3)
GLOBAL_UNCERTAINTY_ASSIGNED_CONTEXT((#17218))
GLOBAL_UNIT_ASSIGNED_CONTEXT((#17323,#17325,#17326))
REPRESENTATION_CONTEXT('','3D')
);
#17280=(
GEOMETRIC_REPRESENTATION_CONTEXT(3)
GLOBAL_UNCERTAINTY_ASSIGNED_CONTEXT((#17219))
GLOBAL_UNIT_ASSIGNED_CONTEXT((#17323,#17325,#17326))
REPRESENTATION_CONTEXT('','3D')
);
#17281=(
GEOMETRIC_REPRESENTATION_CONTEXT(3)
GLOBAL_UNCERTAINTY_ASSIGNED_CONTEXT((#17220))
GLOBAL_UNIT_ASSIGNED_CONTEXT((#17323,#17325,#17326))
REPRESENTATION_CONTEXT('','3D')
);
#17282=(
GEOMETRIC_REPRESENTATION_CONTEXT(3)
GLOBAL_UNCERTAINTY_ASSIGNED_CONTEXT((#17221))
GLOBAL_UNIT_ASSIGNED_CONTEXT((#17323,#17325,#17326))
REPRESENTATION_CONTEXT('','3D')
);
#17283=(
GEOMETRIC_REPRESENTATION_CONTEXT(3)
GLOBAL_UNCERTAINTY_ASSIGNED_CONTEXT((#17222))
GLOBAL_UNIT_ASSIGNED_CONTEXT((#17323,#17325,#17326))
REPRESENTATION_CONTEXT('','3D')
);
#17284=(
GEOMETRIC_REPRESENTATION_CONTEXT(3)
GLOBAL_UNCERTAINTY_ASSIGNED_CONTEXT((#17223))
GLOBAL_UNIT_ASSIGNED_CONTEXT((#17323,#17325,#17326))
REPRESENTATION_CONTEXT('','3D')
);
#17285=(
GEOMETRIC_REPRESENTATION_CONTEXT(3)
GLOBAL_UNCERTAINTY_ASSIGNED_CONTEXT((#17224))
GLOBAL_UNIT_ASSIGNED_CONTEXT((#17323,#17325,#17326))
REPRESENTATION_CONTEXT('','3D')
);
#17286=(
GEOMETRIC_REPRESENTATION_CONTEXT(3)
GLOBAL_UNCERTAINTY_ASSIGNED_CONTEXT((#17225))
GLOBAL_UNIT_ASSIGNED_CONTEXT((#17323,#17325,#17326))
REPRESENTATION_CONTEXT('','3D')
);
#17287=(
GEOMETRIC_REPRESENTATION_CONTEXT(3)
GLOBAL_UNCERTAINTY_ASSIGNED_CONTEXT((#17226))
GLOBAL_UNIT_ASSIGNED_CONTEXT((#17323,#17325,#17326))
REPRESENTATION_CONTEXT('','3D')
);
#17288=(
GEOMETRIC_REPRESENTATION_CONTEXT(3)
GLOBAL_UNCERTAINTY_ASSIGNED_CONTEXT((#17227))
GLOBAL_UNIT_ASSIGNED_CONTEXT((#17323,#17325,#17326))
REPRESENTATION_CONTEXT('','3D')
);
#17289=(
GEOMETRIC_REPRESENTATION_CONTEXT(3)
GLOBAL_UNCERTAINTY_ASSIGNED_CONTEXT((#17228))
GLOBAL_UNIT_ASSIGNED_CONTEXT((#17323,#17325,#17326))
REPRESENTATION_CONTEXT('','3D')
);
#17290=(
GEOMETRIC_REPRESENTATION_CONTEXT(3)
GLOBAL_UNCERTAINTY_ASSIGNED_CONTEXT((#17229))
GLOBAL_UNIT_ASSIGNED_CONTEXT((#17323,#17325,#17326))
REPRESENTATION_CONTEXT('','3D')
);
#17291=(
GEOMETRIC_REPRESENTATION_CONTEXT(3)
GLOBAL_UNCERTAINTY_ASSIGNED_CONTEXT((#17230))
GLOBAL_UNIT_ASSIGNED_CONTEXT((#17323,#17325,#17326))
REPRESENTATION_CONTEXT('','3D')
);
#17292=(
GEOMETRIC_REPRESENTATION_CONTEXT(3)
GLOBAL_UNCERTAINTY_ASSIGNED_CONTEXT((#17231))
GLOBAL_UNIT_ASSIGNED_CONTEXT((#17323,#17325,#17326))
REPRESENTATION_CONTEXT('','3D')
);
#17293=(
GEOMETRIC_REPRESENTATION_CONTEXT(3)
GLOBAL_UNCERTAINTY_ASSIGNED_CONTEXT((#17232))
GLOBAL_UNIT_ASSIGNED_CONTEXT((#17323,#17325,#17326))
REPRESENTATION_CONTEXT('','3D')
);
#17294=(
GEOMETRIC_REPRESENTATION_CONTEXT(3)
GLOBAL_UNCERTAINTY_ASSIGNED_CONTEXT((#17233))
GLOBAL_UNIT_ASSIGNED_CONTEXT((#17323,#17325,#17326))
REPRESENTATION_CONTEXT('','3D')
);
#17295=(
GEOMETRIC_REPRESENTATION_CONTEXT(3)
GLOBAL_UNCERTAINTY_ASSIGNED_CONTEXT((#17234))
GLOBAL_UNIT_ASSIGNED_CONTEXT((#17323,#17325,#17326))
REPRESENTATION_CONTEXT('','3D')
);
#17296=(
GEOMETRIC_REPRESENTATION_CONTEXT(3)
GLOBAL_UNCERTAINTY_ASSIGNED_CONTEXT((#17235))
GLOBAL_UNIT_ASSIGNED_CONTEXT((#17323,#17325,#17326))
REPRESENTATION_CONTEXT('','3D')
);
#17297=(
GEOMETRIC_REPRESENTATION_CONTEXT(3)
GLOBAL_UNCERTAINTY_ASSIGNED_CONTEXT((#17236))
GLOBAL_UNIT_ASSIGNED_CONTEXT((#17323,#17325,#17326))
REPRESENTATION_CONTEXT('','3D')
);
#17298=(
GEOMETRIC_REPRESENTATION_CONTEXT(3)
GLOBAL_UNCERTAINTY_ASSIGNED_CONTEXT((#17237))
GLOBAL_UNIT_ASSIGNED_CONTEXT((#17323,#17325,#17326))
REPRESENTATION_CONTEXT('','3D')
);
#17299=(
GEOMETRIC_REPRESENTATION_CONTEXT(3)
GLOBAL_UNCERTAINTY_ASSIGNED_CONTEXT((#17238))
GLOBAL_UNIT_ASSIGNED_CONTEXT((#17323,#17325,#17326))
REPRESENTATION_CONTEXT('','3D')
);
#17300=(
GEOMETRIC_REPRESENTATION_CONTEXT(3)
GLOBAL_UNCERTAINTY_ASSIGNED_CONTEXT((#17239))
GLOBAL_UNIT_ASSIGNED_CONTEXT((#17323,#17325,#17326))
REPRESENTATION_CONTEXT('','3D')
);
#17301=(
GEOMETRIC_REPRESENTATION_CONTEXT(3)
GLOBAL_UNCERTAINTY_ASSIGNED_CONTEXT((#17240))
GLOBAL_UNIT_ASSIGNED_CONTEXT((#17323,#17325,#17326))
REPRESENTATION_CONTEXT('','3D')
);
#17302=(
GEOMETRIC_REPRESENTATION_CONTEXT(3)
GLOBAL_UNCERTAINTY_ASSIGNED_CONTEXT((#17241))
GLOBAL_UNIT_ASSIGNED_CONTEXT((#17323,#17325,#17326))
REPRESENTATION_CONTEXT('','3D')
);
#17303=(
GEOMETRIC_REPRESENTATION_CONTEXT(3)
GLOBAL_UNCERTAINTY_ASSIGNED_CONTEXT((#17242))
GLOBAL_UNIT_ASSIGNED_CONTEXT((#17323,#17325,#17326))
REPRESENTATION_CONTEXT('','3D')
);
#17304=(
GEOMETRIC_REPRESENTATION_CONTEXT(3)
GLOBAL_UNCERTAINTY_ASSIGNED_CONTEXT((#17243))
GLOBAL_UNIT_ASSIGNED_CONTEXT((#17323,#17325,#17326))
REPRESENTATION_CONTEXT('','3D')
);
#17305=(
GEOMETRIC_REPRESENTATION_CONTEXT(3)
GLOBAL_UNCERTAINTY_ASSIGNED_CONTEXT((#17244))
GLOBAL_UNIT_ASSIGNED_CONTEXT((#17323,#17325,#17326))
REPRESENTATION_CONTEXT('','3D')
);
#17306=(
GEOMETRIC_REPRESENTATION_CONTEXT(3)
GLOBAL_UNCERTAINTY_ASSIGNED_CONTEXT((#17245))
GLOBAL_UNIT_ASSIGNED_CONTEXT((#17323,#17325,#17326))
REPRESENTATION_CONTEXT('','3D')
);
#17307=(
GEOMETRIC_REPRESENTATION_CONTEXT(3)
GLOBAL_UNCERTAINTY_ASSIGNED_CONTEXT((#17246))
GLOBAL_UNIT_ASSIGNED_CONTEXT((#17323,#17325,#17326))
REPRESENTATION_CONTEXT('','3D')
);
#17308=(
GEOMETRIC_REPRESENTATION_CONTEXT(3)
GLOBAL_UNCERTAINTY_ASSIGNED_CONTEXT((#17247))
GLOBAL_UNIT_ASSIGNED_CONTEXT((#17323,#17325,#17326))
REPRESENTATION_CONTEXT('','3D')
);
#17309=(
GEOMETRIC_REPRESENTATION_CONTEXT(3)
GLOBAL_UNCERTAINTY_ASSIGNED_CONTEXT((#17248))
GLOBAL_UNIT_ASSIGNED_CONTEXT((#17323,#17325,#17326))
REPRESENTATION_CONTEXT('','3D')
);
#17310=(
GEOMETRIC_REPRESENTATION_CONTEXT(3)
GLOBAL_UNCERTAINTY_ASSIGNED_CONTEXT((#17249))
GLOBAL_UNIT_ASSIGNED_CONTEXT((#17323,#17325,#17326))
REPRESENTATION_CONTEXT('','3D')
);
#17311=(
GEOMETRIC_REPRESENTATION_CONTEXT(3)
GLOBAL_UNCERTAINTY_ASSIGNED_CONTEXT((#17250))
GLOBAL_UNIT_ASSIGNED_CONTEXT((#17323,#17325,#17326))
REPRESENTATION_CONTEXT('','3D')
);
#17312=(
GEOMETRIC_REPRESENTATION_CONTEXT(3)
GLOBAL_UNCERTAINTY_ASSIGNED_CONTEXT((#17251))
GLOBAL_UNIT_ASSIGNED_CONTEXT((#17323,#17325,#17326))
REPRESENTATION_CONTEXT('','3D')
);
#17313=(
GEOMETRIC_REPRESENTATION_CONTEXT(3)
GLOBAL_UNCERTAINTY_ASSIGNED_CONTEXT((#17252))
GLOBAL_UNIT_ASSIGNED_CONTEXT((#17323,#17325,#17326))
REPRESENTATION_CONTEXT('','3D')
);
#17314=(
GEOMETRIC_REPRESENTATION_CONTEXT(3)
GLOBAL_UNCERTAINTY_ASSIGNED_CONTEXT((#17253))
GLOBAL_UNIT_ASSIGNED_CONTEXT((#17323,#17325,#17326))
REPRESENTATION_CONTEXT('','3D')
);
#17315=(
GEOMETRIC_REPRESENTATION_CONTEXT(3)
GLOBAL_UNCERTAINTY_ASSIGNED_CONTEXT((#17254))
GLOBAL_UNIT_ASSIGNED_CONTEXT((#17323,#17325,#17326))
REPRESENTATION_CONTEXT('','3D')
);
#17316=(
GEOMETRIC_REPRESENTATION_CONTEXT(3)
GLOBAL_UNCERTAINTY_ASSIGNED_CONTEXT((#17255))
GLOBAL_UNIT_ASSIGNED_CONTEXT((#17323,#17325,#17326))
REPRESENTATION_CONTEXT('','3D')
);
#17317=(
GEOMETRIC_REPRESENTATION_CONTEXT(3)
GLOBAL_UNCERTAINTY_ASSIGNED_CONTEXT((#17256))
GLOBAL_UNIT_ASSIGNED_CONTEXT((#17323,#17325,#17326))
REPRESENTATION_CONTEXT('','3D')
);
#17318=(
GEOMETRIC_REPRESENTATION_CONTEXT(3)
GLOBAL_UNCERTAINTY_ASSIGNED_CONTEXT((#17257))
GLOBAL_UNIT_ASSIGNED_CONTEXT((#17323,#17325,#17326))
REPRESENTATION_CONTEXT('','3D')
);
#17319=(
GEOMETRIC_REPRESENTATION_CONTEXT(3)
GLOBAL_UNCERTAINTY_ASSIGNED_CONTEXT((#17258))
GLOBAL_UNIT_ASSIGNED_CONTEXT((#17323,#17325,#17326))
REPRESENTATION_CONTEXT('','3D')
);
#17320=(
GEOMETRIC_REPRESENTATION_CONTEXT(3)
GLOBAL_UNCERTAINTY_ASSIGNED_CONTEXT((#17259))
GLOBAL_UNIT_ASSIGNED_CONTEXT((#17323,#17325,#17326))
REPRESENTATION_CONTEXT('','3D')
);
#17321=(
GEOMETRIC_REPRESENTATION_CONTEXT(3)
GLOBAL_UNCERTAINTY_ASSIGNED_CONTEXT((#17260))
GLOBAL_UNIT_ASSIGNED_CONTEXT((#17323,#17325,#17326))
REPRESENTATION_CONTEXT('','3D')
);
#17322=(
GEOMETRIC_REPRESENTATION_CONTEXT(3)
GLOBAL_UNCERTAINTY_ASSIGNED_CONTEXT((#17261))
GLOBAL_UNIT_ASSIGNED_CONTEXT((#17323,#17325,#17326))
REPRESENTATION_CONTEXT('','3D')
);
#17323=(
LENGTH_UNIT()
NAMED_UNIT(*)
SI_UNIT(.CENTI.,.METRE.)
);
#17324=(
LENGTH_UNIT()
NAMED_UNIT(*)
SI_UNIT($,.METRE.)
);
#17325=(
NAMED_UNIT(*)
PLANE_ANGLE_UNIT()
SI_UNIT($,.RADIAN.)
);
#17326=(
NAMED_UNIT(*)
SI_UNIT($,.STERADIAN.)
SOLID_ANGLE_UNIT()
);
#17327=SHAPE_DEFINITION_REPRESENTATION(#17387,#17558);
#17328=SHAPE_DEFINITION_REPRESENTATION(#17388,#17559);
#17329=SHAPE_DEFINITION_REPRESENTATION(#17389,#17560);
#17330=SHAPE_DEFINITION_REPRESENTATION(#17390,#17561);
#17331=SHAPE_DEFINITION_REPRESENTATION(#17391,#17562);
#17332=SHAPE_DEFINITION_REPRESENTATION(#17392,#17563);
#17333=SHAPE_DEFINITION_REPRESENTATION(#17393,#17564);
#17334=SHAPE_DEFINITION_REPRESENTATION(#17394,#17565);
#17335=SHAPE_DEFINITION_REPRESENTATION(#17395,#17566);
#17336=SHAPE_DEFINITION_REPRESENTATION(#17396,#17567);
#17337=SHAPE_DEFINITION_REPRESENTATION(#17397,#17568);
#17338=SHAPE_DEFINITION_REPRESENTATION(#17398,#17569);
#17339=SHAPE_DEFINITION_REPRESENTATION(#17399,#17570);
#17340=SHAPE_DEFINITION_REPRESENTATION(#17400,#17571);
#17341=SHAPE_DEFINITION_REPRESENTATION(#17401,#17572);
#17342=SHAPE_DEFINITION_REPRESENTATION(#17402,#17573);
#17343=SHAPE_DEFINITION_REPRESENTATION(#17403,#17574);
#17344=SHAPE_DEFINITION_REPRESENTATION(#17406,#17575);
#17345=SHAPE_DEFINITION_REPRESENTATION(#17407,#17576);
#17346=SHAPE_DEFINITION_REPRESENTATION(#17408,#17577);
#17347=SHAPE_DEFINITION_REPRESENTATION(#17409,#17578);
#17348=SHAPE_DEFINITION_REPRESENTATION(#17410,#17579);
#17349=SHAPE_DEFINITION_REPRESENTATION(#17411,#17580);
#17350=SHAPE_DEFINITION_REPRESENTATION(#17412,#17581);
#17351=SHAPE_DEFINITION_REPRESENTATION(#17413,#17582);
#17352=SHAPE_DEFINITION_REPRESENTATION(#17414,#17583);
#17353=SHAPE_DEFINITION_REPRESENTATION(#17415,#17584);
#17354=SHAPE_DEFINITION_REPRESENTATION(#17416,#17585);
#17355=SHAPE_DEFINITION_REPRESENTATION(#17417,#17586);
#17356=SHAPE_DEFINITION_REPRESENTATION(#17418,#17587);
#17357=SHAPE_DEFINITION_REPRESENTATION(#17419,#17588);
#17358=SHAPE_DEFINITION_REPRESENTATION(#17420,#17589);
#17359=SHAPE_DEFINITION_REPRESENTATION(#17421,#17590);
#17360=SHAPE_DEFINITION_REPRESENTATION(#17422,#17591);
#17361=SHAPE_DEFINITION_REPRESENTATION(#17423,#17592);
#17362=SHAPE_DEFINITION_REPRESENTATION(#17424,#17593);
#17363=SHAPE_DEFINITION_REPRESENTATION(#17425,#17594);
#17364=SHAPE_DEFINITION_REPRESENTATION(#17426,#17595);
#17365=SHAPE_DEFINITION_REPRESENTATION(#17427,#17596);
#17366=SHAPE_DEFINITION_REPRESENTATION(#17428,#17597);
#17367=SHAPE_DEFINITION_REPRESENTATION(#17429,#17598);
#17368=SHAPE_DEFINITION_REPRESENTATION(#17430,#17599);
#17369=SHAPE_DEFINITION_REPRESENTATION(#17431,#17600);
#17370=SHAPE_DEFINITION_REPRESENTATION(#17432,#17601);
#17371=SHAPE_DEFINITION_REPRESENTATION(#17433,#17602);
#17372=SHAPE_DEFINITION_REPRESENTATION(#17434,#17603);
#17373=SHAPE_DEFINITION_REPRESENTATION(#17435,#17604);
#17374=SHAPE_DEFINITION_REPRESENTATION(#17436,#17605);
#17375=SHAPE_DEFINITION_REPRESENTATION(#17449,#17606);
#17376=SHAPE_DEFINITION_REPRESENTATION(#17450,#17607);
#17377=SHAPE_DEFINITION_REPRESENTATION(#17451,#17608);
#17378=SHAPE_DEFINITION_REPRESENTATION(#17452,#17609);
#17379=SHAPE_DEFINITION_REPRESENTATION(#17453,#17610);
#17380=SHAPE_DEFINITION_REPRESENTATION(#17454,#17611);
#17381=SHAPE_DEFINITION_REPRESENTATION(#17455,#17612);
#17382=SHAPE_DEFINITION_REPRESENTATION(#17456,#17613);
#17383=SHAPE_DEFINITION_REPRESENTATION(#17457,#17614);
#17384=SHAPE_DEFINITION_REPRESENTATION(#17458,#17615);
#17385=SHAPE_DEFINITION_REPRESENTATION(#17459,#17616);
#17386=SHAPE_DEFINITION_REPRESENTATION(#17462,#17617);
#17387=PRODUCT_DEFINITION_SHAPE('',$,#17619);
#17388=PRODUCT_DEFINITION_SHAPE('',$,#17620);
#17389=PRODUCT_DEFINITION_SHAPE('',$,#17621);
#17390=PRODUCT_DEFINITION_SHAPE('',$,#17622);
#17391=PRODUCT_DEFINITION_SHAPE('',$,#17623);
#17392=PRODUCT_DEFINITION_SHAPE('',$,#17624);
#17393=PRODUCT_DEFINITION_SHAPE('',$,#17625);
#17394=PRODUCT_DEFINITION_SHAPE('',$,#17626);
#17395=PRODUCT_DEFINITION_SHAPE('',$,#17627);
#17396=PRODUCT_DEFINITION_SHAPE('',$,#17628);
#17397=PRODUCT_DEFINITION_SHAPE('',$,#17629);
#17398=PRODUCT_DEFINITION_SHAPE('',$,#17630);
#17399=PRODUCT_DEFINITION_SHAPE('',$,#17631);
#17400=PRODUCT_DEFINITION_SHAPE('',$,#17632);
#17401=PRODUCT_DEFINITION_SHAPE('',$,#17633);
#17402=PRODUCT_DEFINITION_SHAPE('',$,#17634);
#17403=PRODUCT_DEFINITION_SHAPE('',$,#17635);
#17404=PRODUCT_DEFINITION_SHAPE($,$,#346);
#17405=PRODUCT_DEFINITION_SHAPE($,$,#347);
#17406=PRODUCT_DEFINITION_SHAPE('',$,#17636);
#17407=PRODUCT_DEFINITION_SHAPE('',$,#17637);
#17408=PRODUCT_DEFINITION_SHAPE('',$,#17638);
#17409=PRODUCT_DEFINITION_SHAPE('',$,#17639);
#17410=PRODUCT_DEFINITION_SHAPE('',$,#17640);
#17411=PRODUCT_DEFINITION_SHAPE('',$,#17641);
#17412=PRODUCT_DEFINITION_SHAPE('',$,#17642);
#17413=PRODUCT_DEFINITION_SHAPE('',$,#17643);
#17414=PRODUCT_DEFINITION_SHAPE('',$,#17644);
#17415=PRODUCT_DEFINITION_SHAPE('',$,#17645);
#17416=PRODUCT_DEFINITION_SHAPE('',$,#17646);
#17417=PRODUCT_DEFINITION_SHAPE('',$,#17647);
#17418=PRODUCT_DEFINITION_SHAPE('',$,#17648);
#17419=PRODUCT_DEFINITION_SHAPE('',$,#17649);
#17420=PRODUCT_DEFINITION_SHAPE('',$,#17650);
#17421=PRODUCT_DEFINITION_SHAPE('',$,#17651);
#17422=PRODUCT_DEFINITION_SHAPE('',$,#17652);
#17423=PRODUCT_DEFINITION_SHAPE('',$,#17653);
#17424=PRODUCT_DEFINITION_SHAPE('',$,#17654);
#17425=PRODUCT_DEFINITION_SHAPE('',$,#17655);
#17426=PRODUCT_DEFINITION_SHAPE('',$,#17656);
#17427=PRODUCT_DEFINITION_SHAPE('',$,#17657);
#17428=PRODUCT_DEFINITION_SHAPE('',$,#17658);
#17429=PRODUCT_DEFINITION_SHAPE('',$,#17659);
#17430=PRODUCT_DEFINITION_SHAPE('',$,#17660);
#17431=PRODUCT_DEFINITION_SHAPE('',$,#17661);
#17432=PRODUCT_DEFINITION_SHAPE('',$,#17662);
#17433=PRODUCT_DEFINITION_SHAPE('',$,#17663);
#17434=PRODUCT_DEFINITION_SHAPE('',$,#17664);
#17435=PRODUCT_DEFINITION_SHAPE('',$,#17665);
#17436=PRODUCT_DEFINITION_SHAPE('',$,#17666);
#17437=PRODUCT_DEFINITION_SHAPE($,$,#348);
#17438=PRODUCT_DEFINITION_SHAPE($,$,#349);
#17439=PRODUCT_DEFINITION_SHAPE($,$,#350);
#17440=PRODUCT_DEFINITION_SHAPE($,$,#351);
#17441=PRODUCT_DEFINITION_SHAPE($,$,#352);
#17442=PRODUCT_DEFINITION_SHAPE($,$,#353);
#17443=PRODUCT_DEFINITION_SHAPE($,$,#354);
#17444=PRODUCT_DEFINITION_SHAPE($,$,#355);
#17445=PRODUCT_DEFINITION_SHAPE($,$,#356);
#17446=PRODUCT_DEFINITION_SHAPE($,$,#357);
#17447=PRODUCT_DEFINITION_SHAPE($,$,#358);
#17448=PRODUCT_DEFINITION_SHAPE($,$,#359);
#17449=PRODUCT_DEFINITION_SHAPE('',$,#17667);
#17450=PRODUCT_DEFINITION_SHAPE('',$,#17668);
#17451=PRODUCT_DEFINITION_SHAPE('',$,#17669);
#17452=PRODUCT_DEFINITION_SHAPE('',$,#17670);
#17453=PRODUCT_DEFINITION_SHAPE('',$,#17671);
#17454=PRODUCT_DEFINITION_SHAPE('',$,#17672);
#17455=PRODUCT_DEFINITION_SHAPE('',$,#17673);
#17456=PRODUCT_DEFINITION_SHAPE('',$,#17674);
#17457=PRODUCT_DEFINITION_SHAPE('',$,#17675);
#17458=PRODUCT_DEFINITION_SHAPE('',$,#17676);
#17459=PRODUCT_DEFINITION_SHAPE('',$,#17677);
#17460=PRODUCT_DEFINITION_SHAPE($,$,#360);
#17461=PRODUCT_DEFINITION_SHAPE($,$,#361);
#17462=PRODUCT_DEFINITION_SHAPE('',$,#17678);
#17463=PRODUCT_DEFINITION_SHAPE($,$,#362);
#17464=PRODUCT_DEFINITION_SHAPE($,$,#363);
#17465=PRODUCT_DEFINITION_SHAPE($,$,#364);
#17466=PRODUCT_DEFINITION_SHAPE($,$,#365);
#17467=PRODUCT_DEFINITION_SHAPE($,$,#366);
#17468=PRODUCT_DEFINITION_SHAPE($,$,#367);
#17469=PRODUCT_DEFINITION_SHAPE($,$,#368);
#17470=PRODUCT_DEFINITION_SHAPE($,$,#369);
#17471=PRODUCT_DEFINITION_SHAPE($,$,#370);
#17472=PRODUCT_DEFINITION_SHAPE($,$,#371);
#17473=PRODUCT_DEFINITION_SHAPE($,$,#372);
#17474=PRODUCT_DEFINITION_SHAPE($,$,#373);
#17475=PRODUCT_DEFINITION_SHAPE($,$,#374);
#17476=PRODUCT_DEFINITION_SHAPE($,$,#375);
#17477=PRODUCT_DEFINITION_SHAPE($,$,#376);
#17478=PRODUCT_DEFINITION_SHAPE($,$,#377);
#17479=PRODUCT_DEFINITION_SHAPE($,$,#378);
#17480=PRODUCT_DEFINITION_SHAPE($,$,#379);
#17481=PRODUCT_DEFINITION_SHAPE($,$,#380);
#17482=PRODUCT_DEFINITION_SHAPE($,$,#381);
#17483=PRODUCT_DEFINITION_SHAPE($,$,#382);
#17484=PRODUCT_DEFINITION_SHAPE($,$,#383);
#17485=PRODUCT_DEFINITION_SHAPE($,$,#384);
#17486=PRODUCT_DEFINITION_SHAPE($,$,#385);
#17487=PRODUCT_DEFINITION_SHAPE($,$,#386);
#17488=PRODUCT_DEFINITION_SHAPE($,$,#387);
#17489=PRODUCT_DEFINITION_SHAPE($,$,#388);
#17490=PRODUCT_DEFINITION_SHAPE($,$,#389);
#17491=PRODUCT_DEFINITION_SHAPE($,$,#390);
#17492=PRODUCT_DEFINITION_SHAPE($,$,#391);
#17493=PRODUCT_DEFINITION_SHAPE($,$,#392);
#17494=PRODUCT_DEFINITION_SHAPE($,$,#393);
#17495=PRODUCT_DEFINITION_SHAPE($,$,#394);
#17496=PRODUCT_DEFINITION_SHAPE($,$,#395);
#17497=PRODUCT_DEFINITION_SHAPE($,$,#396);
#17498=PRODUCT_DEFINITION_SHAPE($,$,#397);
#17499=PRODUCT_DEFINITION_SHAPE($,$,#398);
#17500=PRODUCT_DEFINITION_SHAPE($,$,#399);
#17501=PRODUCT_DEFINITION_SHAPE($,$,#400);
#17502=PRODUCT_DEFINITION_SHAPE($,$,#401);
#17503=PRODUCT_DEFINITION_SHAPE($,$,#402);
#17504=PRODUCT_DEFINITION_SHAPE($,$,#403);
#17505=PRODUCT_DEFINITION_SHAPE($,$,#404);
#17506=PRODUCT_DEFINITION_SHAPE($,$,#405);
#17507=PRODUCT_DEFINITION_SHAPE($,$,#406);
#17508=PRODUCT_DEFINITION_SHAPE($,$,#407);
#17509=PRODUCT_DEFINITION_SHAPE($,$,#408);
#17510=PRODUCT_DEFINITION_SHAPE($,$,#409);
#17511=PRODUCT_DEFINITION_SHAPE($,$,#410);
#17512=PRODUCT_DEFINITION_SHAPE($,$,#411);
#17513=PRODUCT_DEFINITION_SHAPE($,$,#412);
#17514=PRODUCT_DEFINITION_SHAPE($,$,#413);
#17515=PRODUCT_DEFINITION_SHAPE($,$,#414);
#17516=PRODUCT_DEFINITION_SHAPE($,$,#415);
#17517=PRODUCT_DEFINITION_SHAPE($,$,#416);
#17518=PRODUCT_DEFINITION_SHAPE($,$,#417);
#17519=PRODUCT_DEFINITION_SHAPE($,$,#418);
#17520=PRODUCT_DEFINITION_SHAPE($,$,#419);
#17521=PRODUCT_DEFINITION_SHAPE($,$,#420);
#17522=PRODUCT_DEFINITION_SHAPE($,$,#421);
#17523=PRODUCT_DEFINITION_SHAPE($,$,#422);
#17524=PRODUCT_DEFINITION_SHAPE($,$,#423);
#17525=PRODUCT_DEFINITION_SHAPE($,$,#424);
#17526=PRODUCT_DEFINITION_SHAPE($,$,#425);
#17527=PRODUCT_DEFINITION_SHAPE($,$,#426);
#17528=PRODUCT_DEFINITION_SHAPE($,$,#427);
#17529=PRODUCT_DEFINITION_SHAPE($,$,#428);
#17530=PRODUCT_DEFINITION_SHAPE($,$,#429);
#17531=PRODUCT_DEFINITION_SHAPE($,$,#430);
#17532=PRODUCT_DEFINITION_SHAPE($,$,#431);
#17533=PRODUCT_DEFINITION_SHAPE($,$,#432);
#17534=PRODUCT_DEFINITION_SHAPE($,$,#433);
#17535=PRODUCT_DEFINITION_SHAPE($,$,#434);
#17536=PRODUCT_DEFINITION_SHAPE($,$,#435);
#17537=PRODUCT_DEFINITION_SHAPE($,$,#436);
#17538=PRODUCT_DEFINITION_SHAPE($,$,#437);
#17539=PRODUCT_DEFINITION_SHAPE($,$,#438);
#17540=PRODUCT_DEFINITION_SHAPE($,$,#439);
#17541=PRODUCT_DEFINITION_SHAPE($,$,#440);
#17542=PRODUCT_DEFINITION_SHAPE($,$,#441);
#17543=PRODUCT_DEFINITION_SHAPE($,$,#442);
#17544=PRODUCT_DEFINITION_SHAPE($,$,#443);
#17545=PRODUCT_DEFINITION_SHAPE($,$,#444);
#17546=PRODUCT_DEFINITION_SHAPE($,$,#445);
#17547=PRODUCT_DEFINITION_SHAPE($,$,#446);
#17548=PRODUCT_DEFINITION_SHAPE($,$,#447);
#17549=PRODUCT_DEFINITION_SHAPE($,$,#448);
#17550=PRODUCT_DEFINITION_SHAPE($,$,#449);
#17551=PRODUCT_DEFINITION_SHAPE($,$,#450);
#17552=PRODUCT_DEFINITION_SHAPE($,$,#451);
#17553=PRODUCT_DEFINITION_SHAPE($,$,#452);
#17554=PRODUCT_DEFINITION_SHAPE($,$,#453);
#17555=PRODUCT_DEFINITION_SHAPE($,$,#454);
#17556=PRODUCT_DEFINITION_SHAPE($,$,#455);
#17557=PRODUCT_DEFINITION_SHAPE($,$,#456);
#17558=SHAPE_REPRESENTATION('',(#9685,#10826,#10827,#10828,#10829),#17262);
#17559=SHAPE_REPRESENTATION('',(#9686,#10735,#10736,#10737,#10738,#10739,
#10740,#10741,#10742,#10743,#10744,#10745,#10746,#10747,#10748,#10749,#10750,
#10751,#10752,#10753,#10754,#10755,#10756,#10757,#10758,#10759,#10760,#10761,
#10762,#10763,#10764,#10765,#10766,#10767,#10768,#10769,#10770,#10771,#10772,
#10773,#10774,#10775,#10776,#10777,#10778,#10779,#10780,#10781,#10782,#10783,
#10784,#10785,#10786,#10787,#10788,#10789,#10790,#10791,#10792,#10793),
#17263);
#17560=SHAPE_REPRESENTATION('',(#9687),#17264);
#17561=SHAPE_REPRESENTATION('',(#9730),#17265);
#17562=SHAPE_REPRESENTATION('',(#9773),#17266);
#17563=SHAPE_REPRESENTATION('',(#9782),#17267);
#17564=SHAPE_REPRESENTATION('',(#9791),#17268);
#17565=SHAPE_REPRESENTATION('',(#9834),#17269);
#17566=SHAPE_REPRESENTATION('',(#9843),#17270);
#17567=SHAPE_REPRESENTATION('',(#9852),#17271);
#17568=SHAPE_REPRESENTATION('',(#9892),#17272);
#17569=SHAPE_REPRESENTATION('',(#9932),#17273);
#17570=SHAPE_REPRESENTATION('',(#9939),#17274);
#17571=SHAPE_REPRESENTATION('',(#9946),#17275);
#17572=SHAPE_REPRESENTATION('',(#9972,#10042,#10043),#17276);
#17573=SHAPE_REPRESENTATION('',(#9973),#17277);
#17574=SHAPE_REPRESENTATION('',(#10014),#17278);
#17575=SHAPE_REPRESENTATION('',(#10044),#17279);
#17576=SHAPE_REPRESENTATION('',(#10053),#17280);
#17577=SHAPE_REPRESENTATION('',(#10077),#17281);
#17578=SHAPE_REPRESENTATION('',(#10115),#17282);
#17579=SHAPE_REPRESENTATION('',(#10126),#17283);
#17580=SHAPE_REPRESENTATION('',(#10150),#17284);
#17581=SHAPE_REPRESENTATION('',(#10176),#17285);
#17582=SHAPE_REPRESENTATION('',(#10184,#10794,#10795,#10796,#10797,#10798,
#10799,#10800,#10801,#10802,#10803,#10804,#10805,#10806,#10807),#17286);
#17583=SHAPE_REPRESENTATION('',(#10185),#17287);
#17584=SHAPE_REPRESENTATION('',(#10197),#17288);
#17585=SHAPE_REPRESENTATION('',(#10212),#17289);
#17586=SHAPE_REPRESENTATION('',(#10227),#17290);
#17587=SHAPE_REPRESENTATION('',(#10236),#17291);
#17588=SHAPE_REPRESENTATION('',(#10270),#17292);
#17589=SHAPE_REPRESENTATION('',(#10284),#17293);
#17590=SHAPE_REPRESENTATION('',(#10293),#17294);
#17591=SHAPE_REPRESENTATION('',(#10302),#17295);
#17592=SHAPE_REPRESENTATION('',(#10311),#17296);
#17593=SHAPE_REPRESENTATION('',(#10322),#17297);
#17594=SHAPE_REPRESENTATION('',(#10339,#10527,#10528,#10529,#10530,#10531,
#10532,#10533),#17298);
#17595=SHAPE_REPRESENTATION('',(#10340),#17299);
#17596=SHAPE_REPRESENTATION('',(#10357),#17300);
#17597=SHAPE_REPRESENTATION('',(#10366),#17301);
#17598=SHAPE_REPRESENTATION('',(#10375),#17302);
#17599=SHAPE_REPRESENTATION('',(#10384),#17303);
#17600=SHAPE_REPRESENTATION('',(#10393,#10522,#10523,#10524,#10525,#10526),
#17304);
#17601=SHAPE_REPRESENTATION('',(#10394),#17305);
#17602=SHAPE_REPRESENTATION('',(#10414),#17306);
#17603=SHAPE_REPRESENTATION('',(#10434),#17307);
#17604=SHAPE_REPRESENTATION('',(#10451),#17308);
#17605=SHAPE_REPRESENTATION('',(#10505),#17309);
#17606=SHAPE_REPRESENTATION('',(#10534,#10808,#10809,#10810,#10811,#10812,
#10813,#10814,#10815,#10816,#10817,#10818,#10819,#10820,#10821,#10822,#10823,
#10824,#10825),#17310);
#17607=SHAPE_REPRESENTATION('',(#10535),#17311);
#17608=SHAPE_REPRESENTATION('',(#10568),#17312);
#17609=SHAPE_REPRESENTATION('',(#10593),#17313);
#17610=SHAPE_REPRESENTATION('',(#10618),#17314);
#17611=SHAPE_REPRESENTATION('',(#10632),#17315);
#17612=SHAPE_REPRESENTATION('',(#10641),#17316);
#17613=SHAPE_REPRESENTATION('',(#10650),#17317);
#17614=SHAPE_REPRESENTATION('',(#10659,#10709,#10710),#17318);
#17615=SHAPE_REPRESENTATION('',(#10660),#17319);
#17616=SHAPE_REPRESENTATION('',(#10692),#17320);
#17617=SHAPE_REPRESENTATION('',(#10711),#17321);
#17618=PRODUCT_DEFINITION_CONTEXT('part definition',#17800,'design');
#17619=PRODUCT_DEFINITION('PAT-037','PAT-037',#17679,#17618);
#17620=PRODUCT_DEFINITION('Bearing and guide frame',
'Bearing and guide frame',#17680,#17618);
#17621=PRODUCT_DEFINITION('Base','Base',#17681,#17618);
#17622=PRODUCT_DEFINITION('Bearing pedestal','Bearing pedestal',#17682,
#17618);
#17623=PRODUCT_DEFINITION('Bearing bolt reducer','Bearing bolt reducer',
#17683,#17618);
#17624=PRODUCT_DEFINITION('Bearing bolt reducer (1)',
'Bearing bolt reducer (1)',#17684,#17618);
#17625=PRODUCT_DEFINITION('Bearing pedestal (1)','Bearing pedestal (1)',#17685,
#17618);
#17626=PRODUCT_DEFINITION('Bearing bolt reducer (2)',
'Bearing bolt reducer (2)',#17686,#17618);
#17627=PRODUCT_DEFINITION('Bearing bolt reducer (3)',
'Bearing bolt reducer (3)',#17687,#17618);
#17628=PRODUCT_DEFINITION('Guide pedestal','Guide pedestal',#17688,#17618);
#17629=PRODUCT_DEFINITION('Guide pedestal (1)','Guide pedestal (1)',#17689,
#17618);
#17630=PRODUCT_DEFINITION('Foot strip','Foot strip',#17690,#17618);
#17631=PRODUCT_DEFINITION('Foot strip (1)','Foot strip (1)',#17691,#17618);
#17632=PRODUCT_DEFINITION('Cap Screw - M5x20','Cap Screw - M5x20',#17692,
#17618);
#17633=PRODUCT_DEFINITION('Pillow Block Bearing - 20 mm Bore',
'Pillow Block Bearing - 20 mm Bore',#17693,#17618);
#17634=PRODUCT_DEFINITION('Housing','Housing',#17694,#17618);
#17635=PRODUCT_DEFINITION('Insert bearing','Insert bearing',#17695,#17618);
#17636=PRODUCT_DEFINITION('Flat Washer - M8','Flat Washer - M8',#17696,
#17618);
#17637=PRODUCT_DEFINITION('M8x25 Bolt','M8x25 Bolt',#17697,#17618);
#17638=PRODUCT_DEFINITION('Shaft Support - 12 mm Bore',
'Shaft Support - 12 mm Bore',#17698,#17618);
#17639=PRODUCT_DEFINITION('Flat Washer - M5','Flat Washer - M5',#17699,
#17618);
#17640=PRODUCT_DEFINITION('M5x14 Cap Screw','M5x14 Cap Screw',#17700,#17618);
#17641=PRODUCT_DEFINITION('Cap Screw - M4x16','Cap Screw - M4x16',#17701,
#17618);
#17642=PRODUCT_DEFINITION('Guide shaft 200 mm','Guide shaft 200 mm',#17702,
#17618);
#17643=PRODUCT_DEFINITION('Flywheel and crank','Flywheel and crank',#17703,
#17618);
#17644=PRODUCT_DEFINITION('Flywheel shaft','Flywheel shaft',#17704,#17618);
#17645=PRODUCT_DEFINITION('Shaft collar','Shaft collar',#17705,#17618);
#17646=PRODUCT_DEFINITION('Shaft collar (1)','Shaft collar (1)',#17706,#17618);
#17647=PRODUCT_DEFINITION('Rear bearing spacer','Rear bearing spacer',#17707,
#17618);
#17648=PRODUCT_DEFINITION('Flywheel','Flywheel',#17708,#17618);
#17649=PRODUCT_DEFINITION('Crank pin','Crank pin',#17709,#17618);
#17650=PRODUCT_DEFINITION('Pin spacer 10 mm','Pin spacer 10 mm',#17710,
#17618);
#17651=PRODUCT_DEFINITION('Pin spacer 4 mm','Pin spacer 4 mm',#17711,#17618);
#17652=PRODUCT_DEFINITION('Pin keeper','Pin keeper',#17712,#17618);
#17653=PRODUCT_DEFINITION('Key 6x6x20','Key 6x6x20',#17713,#17618);
#17654=PRODUCT_DEFINITION('Socket Set Screw - M5x8',
'Socket Set Screw - M5x8',#17714,#17618);
#17655=PRODUCT_DEFINITION('Connecting rod (1)','Connecting rod (1)',#17715,
#17618);
#17656=PRODUCT_DEFINITION('Connecting rod','Connecting rod',#17716,#17618);
#17657=PRODUCT_DEFINITION('Rod bearing retainer','Rod bearing retainer',
#17717,#17618);
#17658=PRODUCT_DEFINITION('Rod bearing retainer (1)',
'Rod bearing retainer (1)',#17718,#17618);
#17659=PRODUCT_DEFINITION('Rod bearing retainer (2)',
'Rod bearing retainer (2)',#17719,#17618);
#17660=PRODUCT_DEFINITION('Rod bearing retainer (3)',
'Rod bearing retainer (3)',#17720,#17618);
#17661=PRODUCT_DEFINITION('Sealed Ball Bearing - 10 x 30 x 9 mm',
'Sealed Ball Bearing - 10 x 30 x 9 mm',#17721,#17618);
#17662=PRODUCT_DEFINITION('Inner ring','Inner ring',#17722,#17618);
#17663=PRODUCT_DEFINITION('Outer ring','Outer ring',#17723,#17618);
#17664=PRODUCT_DEFINITION('Balls','Balls',#17724,#17618);
#17665=PRODUCT_DEFINITION('Cage','Cage',#17725,#17618);
#17666=PRODUCT_DEFINITION('Seals 2RS','Seals 2RS',#17726,#17618);
#17667=PRODUCT_DEFINITION('Guided slider','Guided slider',#17727,#17618);
#17668=PRODUCT_DEFINITION('Slider housing','Slider housing',#17728,#17618);
#17669=PRODUCT_DEFINITION('Bushing cap','Bushing cap',#17729,#17618);
#17670=PRODUCT_DEFINITION('Bushing cap (1)','Bushing cap (1)',#17730,#17618);
#17671=PRODUCT_DEFINITION('Slider pin','Slider pin',#17731,#17618);
#17672=PRODUCT_DEFINITION('Pin spacer 2 mm','Pin spacer 2 mm',#17732,#17618);
#17673=PRODUCT_DEFINITION('Pin spacer 4 mm (1)','Pin spacer 4 mm (1)',#17733,
#17618);
#17674=PRODUCT_DEFINITION('Pin keeper (1)','Pin keeper (1)',#17734,#17618);
#17675=PRODUCT_DEFINITION('Linear Ball Bushing - 12 x 21 x 30 mm',
'Linear Ball Bushing - 12 x 21 x 30 mm',#17735,#17618);
#17676=PRODUCT_DEFINITION('Steel sleeve','Steel sleeve',#17736,#17618);
#17677=PRODUCT_DEFINITION('Ball retainer (plastic)',
'Ball retainer (plastic)',#17737,#17618);
#17678=PRODUCT_DEFINITION('M4x10 Cap Screw','M4x10 Cap Screw',#17738,#17618);
#17679=PRODUCT_DEFINITION_FORMATION('',$,#17802);
#17680=PRODUCT_DEFINITION_FORMATION('',$,#17803);
#17681=PRODUCT_DEFINITION_FORMATION('',$,#17804);
#17682=PRODUCT_DEFINITION_FORMATION('',$,#17805);
#17683=PRODUCT_DEFINITION_FORMATION('',$,#17806);
#17684=PRODUCT_DEFINITION_FORMATION('',$,#17807);
#17685=PRODUCT_DEFINITION_FORMATION('',$,#17808);
#17686=PRODUCT_DEFINITION_FORMATION('',$,#17809);
#17687=PRODUCT_DEFINITION_FORMATION('',$,#17810);
#17688=PRODUCT_DEFINITION_FORMATION('',$,#17811);
#17689=PRODUCT_DEFINITION_FORMATION('',$,#17812);
#17690=PRODUCT_DEFINITION_FORMATION('',$,#17813);
#17691=PRODUCT_DEFINITION_FORMATION('',$,#17814);
#17692=PRODUCT_DEFINITION_FORMATION('',$,#17815);
#17693=PRODUCT_DEFINITION_FORMATION('',$,#17816);
#17694=PRODUCT_DEFINITION_FORMATION('',$,#17817);
#17695=PRODUCT_DEFINITION_FORMATION('',$,#17818);
#17696=PRODUCT_DEFINITION_FORMATION('',$,#17819);
#17697=PRODUCT_DEFINITION_FORMATION('',$,#17820);
#17698=PRODUCT_DEFINITION_FORMATION('',$,#17821);
#17699=PRODUCT_DEFINITION_FORMATION('',$,#17822);
#17700=PRODUCT_DEFINITION_FORMATION('',$,#17823);
#17701=PRODUCT_DEFINITION_FORMATION('',$,#17824);
#17702=PRODUCT_DEFINITION_FORMATION('',$,#17825);
#17703=PRODUCT_DEFINITION_FORMATION('',$,#17826);
#17704=PRODUCT_DEFINITION_FORMATION('',$,#17827);
#17705=PRODUCT_DEFINITION_FORMATION('',$,#17828);
#17706=PRODUCT_DEFINITION_FORMATION('',$,#17829);
#17707=PRODUCT_DEFINITION_FORMATION('',$,#17830);
#17708=PRODUCT_DEFINITION_FORMATION('',$,#17831);
#17709=PRODUCT_DEFINITION_FORMATION('',$,#17832);
#17710=PRODUCT_DEFINITION_FORMATION('',$,#17833);
#17711=PRODUCT_DEFINITION_FORMATION('',$,#17834);
#17712=PRODUCT_DEFINITION_FORMATION('',$,#17835);
#17713=PRODUCT_DEFINITION_FORMATION('',$,#17836);
#17714=PRODUCT_DEFINITION_FORMATION('',$,#17837);
#17715=PRODUCT_DEFINITION_FORMATION('',$,#17838);
#17716=PRODUCT_DEFINITION_FORMATION('',$,#17839);
#17717=PRODUCT_DEFINITION_FORMATION('',$,#17840);
#17718=PRODUCT_DEFINITION_FORMATION('',$,#17841);
#17719=PRODUCT_DEFINITION_FORMATION('',$,#17842);
#17720=PRODUCT_DEFINITION_FORMATION('',$,#17843);
#17721=PRODUCT_DEFINITION_FORMATION('',$,#17844);
#17722=PRODUCT_DEFINITION_FORMATION('',$,#17845);
#17723=PRODUCT_DEFINITION_FORMATION('',$,#17846);
#17724=PRODUCT_DEFINITION_FORMATION('',$,#17847);
#17725=PRODUCT_DEFINITION_FORMATION('',$,#17848);
#17726=PRODUCT_DEFINITION_FORMATION('',$,#17849);
#17727=PRODUCT_DEFINITION_FORMATION('',$,#17850);
#17728=PRODUCT_DEFINITION_FORMATION('',$,#17851);
#17729=PRODUCT_DEFINITION_FORMATION('',$,#17852);
#17730=PRODUCT_DEFINITION_FORMATION('',$,#17853);
#17731=PRODUCT_DEFINITION_FORMATION('',$,#17854);
#17732=PRODUCT_DEFINITION_FORMATION('',$,#17855);
#17733=PRODUCT_DEFINITION_FORMATION('',$,#17856);
#17734=PRODUCT_DEFINITION_FORMATION('',$,#17857);
#17735=PRODUCT_DEFINITION_FORMATION('',$,#17858);
#17736=PRODUCT_DEFINITION_FORMATION('',$,#17859);
#17737=PRODUCT_DEFINITION_FORMATION('',$,#17860);
#17738=PRODUCT_DEFINITION_FORMATION('',$,#17861);
#17739=PRODUCT_RELATED_PRODUCT_CATEGORY('PAT-037','PAT-037',(#17802));
#17740=PRODUCT_RELATED_PRODUCT_CATEGORY('Bearing and guide frame',
'Bearing and guide frame',(#17803));
#17741=PRODUCT_RELATED_PRODUCT_CATEGORY('Base','Base',(#17804));
#17742=PRODUCT_RELATED_PRODUCT_CATEGORY('Bearing pedestal',
'Bearing pedestal',(#17805));
#17743=PRODUCT_RELATED_PRODUCT_CATEGORY('Bearing bolt reducer',
'Bearing bolt reducer',(#17806));
#17744=PRODUCT_RELATED_PRODUCT_CATEGORY('Bearing bolt reducer (1)',
'Bearing bolt reducer (1)',(#17807));
#17745=PRODUCT_RELATED_PRODUCT_CATEGORY('Bearing pedestal (1)',
'Bearing pedestal (1)',(#17808));
#17746=PRODUCT_RELATED_PRODUCT_CATEGORY('Bearing bolt reducer (2)',
'Bearing bolt reducer (2)',(#17809));
#17747=PRODUCT_RELATED_PRODUCT_CATEGORY('Bearing bolt reducer (3)',
'Bearing bolt reducer (3)',(#17810));
#17748=PRODUCT_RELATED_PRODUCT_CATEGORY('Guide pedestal',
'Guide pedestal',(#17811));
#17749=PRODUCT_RELATED_PRODUCT_CATEGORY('Guide pedestal (1)',
'Guide pedestal (1)',(#17812));
#17750=PRODUCT_RELATED_PRODUCT_CATEGORY('Foot strip','Foot strip',(#17813));
#17751=PRODUCT_RELATED_PRODUCT_CATEGORY('Foot strip (1)',
'Foot strip (1)',(#17814));
#17752=PRODUCT_RELATED_PRODUCT_CATEGORY('Cap Screw - M5x20',
'Cap Screw - M5x20',(#17815));
#17753=PRODUCT_RELATED_PRODUCT_CATEGORY(
'Pillow Block Bearing - 20 mm Bore','Pillow Block Bearing - 20 mm Bore',
(#17816));
#17754=PRODUCT_RELATED_PRODUCT_CATEGORY('Housing','Housing',(#17817));
#17755=PRODUCT_RELATED_PRODUCT_CATEGORY('Insert bearing',
'Insert bearing',(#17818));
#17756=PRODUCT_RELATED_PRODUCT_CATEGORY('Flat Washer - M8',
'Flat Washer - M8',(#17819));
#17757=PRODUCT_RELATED_PRODUCT_CATEGORY('M8x25 Bolt','M8x25 Bolt',(#17820));
#17758=PRODUCT_RELATED_PRODUCT_CATEGORY('Shaft Support - 12 mm Bore',
'Shaft Support - 12 mm Bore',(#17821));
#17759=PRODUCT_RELATED_PRODUCT_CATEGORY('Flat Washer - M5',
'Flat Washer - M5',(#17822));
#17760=PRODUCT_RELATED_PRODUCT_CATEGORY('M5x14 Cap Screw',
'M5x14 Cap Screw',(#17823));
#17761=PRODUCT_RELATED_PRODUCT_CATEGORY('Cap Screw - M4x16',
'Cap Screw - M4x16',(#17824));
#17762=PRODUCT_RELATED_PRODUCT_CATEGORY('Guide shaft 200 mm',
'Guide shaft 200 mm',(#17825));
#17763=PRODUCT_RELATED_PRODUCT_CATEGORY('Flywheel and crank',
'Flywheel and crank',(#17826));
#17764=PRODUCT_RELATED_PRODUCT_CATEGORY('Flywheel shaft',
'Flywheel shaft',(#17827));
#17765=PRODUCT_RELATED_PRODUCT_CATEGORY('Shaft collar','Shaft collar',(#17828));
#17766=PRODUCT_RELATED_PRODUCT_CATEGORY('Shaft collar (1)',
'Shaft collar (1)',(#17829));
#17767=PRODUCT_RELATED_PRODUCT_CATEGORY('Rear bearing spacer',
'Rear bearing spacer',(#17830));
#17768=PRODUCT_RELATED_PRODUCT_CATEGORY('Flywheel','Flywheel',(#17831));
#17769=PRODUCT_RELATED_PRODUCT_CATEGORY('Crank pin','Crank pin',(#17832));
#17770=PRODUCT_RELATED_PRODUCT_CATEGORY('Pin spacer 10 mm',
'Pin spacer 10 mm',(#17833));
#17771=PRODUCT_RELATED_PRODUCT_CATEGORY('Pin spacer 4 mm',
'Pin spacer 4 mm',(#17834));
#17772=PRODUCT_RELATED_PRODUCT_CATEGORY('Pin keeper','Pin keeper',(#17835));
#17773=PRODUCT_RELATED_PRODUCT_CATEGORY('Key 6x6x20','Key 6x6x20',(#17836));
#17774=PRODUCT_RELATED_PRODUCT_CATEGORY('Socket Set Screw - M5x8',
'Socket Set Screw - M5x8',(#17837));
#17775=PRODUCT_RELATED_PRODUCT_CATEGORY('Connecting rod (1)',
'Connecting rod (1)',(#17838));
#17776=PRODUCT_RELATED_PRODUCT_CATEGORY('Connecting rod',
'Connecting rod',(#17839));
#17777=PRODUCT_RELATED_PRODUCT_CATEGORY('Rod bearing retainer',
'Rod bearing retainer',(#17840));
#17778=PRODUCT_RELATED_PRODUCT_CATEGORY('Rod bearing retainer (1)',
'Rod bearing retainer (1)',(#17841));
#17779=PRODUCT_RELATED_PRODUCT_CATEGORY('Rod bearing retainer (2)',
'Rod bearing retainer (2)',(#17842));
#17780=PRODUCT_RELATED_PRODUCT_CATEGORY('Rod bearing retainer (3)',
'Rod bearing retainer (3)',(#17843));
#17781=PRODUCT_RELATED_PRODUCT_CATEGORY(
'Sealed Ball Bearing - 10 x 30 x 9 mm',
'Sealed Ball Bearing - 10 x 30 x 9 mm',(#17844));
#17782=PRODUCT_RELATED_PRODUCT_CATEGORY('Inner ring','Inner ring',(#17845));
#17783=PRODUCT_RELATED_PRODUCT_CATEGORY('Outer ring','Outer ring',(#17846));
#17784=PRODUCT_RELATED_PRODUCT_CATEGORY('Balls','Balls',(#17847));
#17785=PRODUCT_RELATED_PRODUCT_CATEGORY('Cage','Cage',(#17848));
#17786=PRODUCT_RELATED_PRODUCT_CATEGORY('Seals 2RS','Seals 2RS',(#17849));
#17787=PRODUCT_RELATED_PRODUCT_CATEGORY('Guided slider','Guided slider',
(#17850));
#17788=PRODUCT_RELATED_PRODUCT_CATEGORY('Slider housing',
'Slider housing',(#17851));
#17789=PRODUCT_RELATED_PRODUCT_CATEGORY('Bushing cap','Bushing cap',(#17852));
#17790=PRODUCT_RELATED_PRODUCT_CATEGORY('Bushing cap (1)',
'Bushing cap (1)',(#17853));
#17791=PRODUCT_RELATED_PRODUCT_CATEGORY('Slider pin','Slider pin',(#17854));
#17792=PRODUCT_RELATED_PRODUCT_CATEGORY('Pin spacer 2 mm',
'Pin spacer 2 mm',(#17855));
#17793=PRODUCT_RELATED_PRODUCT_CATEGORY('Pin spacer 4 mm (1)',
'Pin spacer 4 mm (1)',(#17856));
#17794=PRODUCT_RELATED_PRODUCT_CATEGORY('Pin keeper (1)',
'Pin keeper (1)',(#17857));
#17795=PRODUCT_RELATED_PRODUCT_CATEGORY(
'Linear Ball Bushing - 12 x 21 x 30 mm',
'Linear Ball Bushing - 12 x 21 x 30 mm',(#17858));
#17796=PRODUCT_RELATED_PRODUCT_CATEGORY('Steel sleeve','Steel sleeve',(#17859));
#17797=PRODUCT_RELATED_PRODUCT_CATEGORY('Ball retainer (plastic)',
'Ball retainer (plastic)',(#17860));
#17798=PRODUCT_RELATED_PRODUCT_CATEGORY('M4x10 Cap Screw',
'M4x10 Cap Screw',(#17861));
#17799=APPLICATION_PROTOCOL_DEFINITION('international standard',
'automotive_design',2009,#17800);
#17800=APPLICATION_CONTEXT(
'Core Data for Automotive Mechanical Design Process');
#17801=PRODUCT_CONTEXT('part definition',#17800,'mechanical');
#17802=PRODUCT('PAT-037','PAT-037',
'PAT-037',(#17801));
#17803=PRODUCT('Bearing and guide frame','Bearing and guide frame',
'Bearing and guide frame',(#17801));
#17804=PRODUCT('Base','Base','Base',(#17801));
#17805=PRODUCT('Bearing pedestal','Bearing pedestal','Bearing pedestal',
(#17801));
#17806=PRODUCT('Bearing bolt reducer','Bearing bolt reducer',
'Bearing bolt reducer',(#17801));
#17807=PRODUCT('Bearing bolt reducer (1)','Bearing bolt reducer (1)',
'Bearing bolt reducer (1)',(#17801));
#17808=PRODUCT('Bearing pedestal (1)','Bearing pedestal (1)',
'Bearing pedestal (1)',(#17801));
#17809=PRODUCT('Bearing bolt reducer (2)','Bearing bolt reducer (2)',
'Bearing bolt reducer (2)',(#17801));
#17810=PRODUCT('Bearing bolt reducer (3)','Bearing bolt reducer (3)',
'Bearing bolt reducer (3)',(#17801));
#17811=PRODUCT('Guide pedestal','Guide pedestal','Guide pedestal',(#17801));
#17812=PRODUCT('Guide pedestal (1)','Guide pedestal (1)','Guide pedestal (1)',
(#17801));
#17813=PRODUCT('Foot strip','Foot strip','Foot strip',(#17801));
#17814=PRODUCT('Foot strip (1)','Foot strip (1)','Foot strip (1)',(#17801));
#17815=PRODUCT('Cap Screw - M5x20','Cap Screw - M5x20',
'Cap Screw - M5x20',(#17801));
#17816=PRODUCT('Pillow Block Bearing - 20 mm Bore',
'Pillow Block Bearing - 20 mm Bore','Pillow Block Bearing - 20 mm Bore',
(#17801));
#17817=PRODUCT('Housing','Housing','Housing',(#17801));
#17818=PRODUCT('Insert bearing','Insert bearing','Insert bearing',(#17801));
#17819=PRODUCT('Flat Washer - M8','Flat Washer - M8','Flat Washer - M8',
(#17801));
#17820=PRODUCT('M8x25 Bolt','M8x25 Bolt','M8x25 Bolt',(#17801));
#17821=PRODUCT('Shaft Support - 12 mm Bore',
'Shaft Support - 12 mm Bore','Shaft Support - 12 mm Bore',(#17801));
#17822=PRODUCT('Flat Washer - M5','Flat Washer - M5','Flat Washer - M5',
(#17801));
#17823=PRODUCT('M5x14 Cap Screw','M5x14 Cap Screw','M5x14 Cap Screw',(#17801));
#17824=PRODUCT('Cap Screw - M4x16','Cap Screw - M4x16',
'Cap Screw - M4x16',(#17801));
#17825=PRODUCT('Guide shaft 200 mm','Guide shaft 200 mm',
'Guide shaft 200 mm',(#17801));
#17826=PRODUCT('Flywheel and crank','Flywheel and crank',
'Flywheel and crank',(#17801));
#17827=PRODUCT('Flywheel shaft','Flywheel shaft','Flywheel shaft',(#17801));
#17828=PRODUCT('Shaft collar','Shaft collar','Shaft collar',(#17801));
#17829=PRODUCT('Shaft collar (1)','Shaft collar (1)','Shaft collar (1)',(#17801));
#17830=PRODUCT('Rear bearing spacer','Rear bearing spacer',
'Rear bearing spacer',(#17801));
#17831=PRODUCT('Flywheel','Flywheel','Flywheel',(#17801));
#17832=PRODUCT('Crank pin','Crank pin','Crank pin',(#17801));
#17833=PRODUCT('Pin spacer 10 mm','Pin spacer 10 mm','Pin spacer 10 mm',
(#17801));
#17834=PRODUCT('Pin spacer 4 mm','Pin spacer 4 mm','Pin spacer 4 mm',(#17801));
#17835=PRODUCT('Pin keeper','Pin keeper','Pin keeper',(#17801));
#17836=PRODUCT('Key 6x6x20','Key 6x6x20','Key 6x6x20',(#17801));
#17837=PRODUCT('Socket Set Screw - M5x8','Socket Set Screw - M5x8',
'Socket Set Screw - M5x8',(#17801));
#17838=PRODUCT('Connecting rod (1)','Connecting rod (1)','Connecting rod (1)',(#17801));
#17839=PRODUCT('Connecting rod','Connecting rod','Connecting rod',(#17801));
#17840=PRODUCT('Rod bearing retainer','Rod bearing retainer',
'Rod bearing retainer',(#17801));
#17841=PRODUCT('Rod bearing retainer (1)','Rod bearing retainer (1)',
'Rod bearing retainer (1)',(#17801));
#17842=PRODUCT('Rod bearing retainer (2)','Rod bearing retainer (2)',
'Rod bearing retainer (2)',(#17801));
#17843=PRODUCT('Rod bearing retainer (3)','Rod bearing retainer (3)',
'Rod bearing retainer (3)',(#17801));
#17844=PRODUCT('Sealed Ball Bearing - 10 x 30 x 9 mm',
'Sealed Ball Bearing - 10 x 30 x 9 mm',
'Sealed Ball Bearing - 10 x 30 x 9 mm',(#17801));
#17845=PRODUCT('Inner ring','Inner ring','Inner ring',(#17801));
#17846=PRODUCT('Outer ring','Outer ring','Outer ring',(#17801));
#17847=PRODUCT('Balls','Balls','Balls',(#17801));
#17848=PRODUCT('Cage','Cage','Cage',(#17801));
#17849=PRODUCT('Seals 2RS','Seals 2RS','Seals 2RS',(#17801));
#17850=PRODUCT('Guided slider','Guided slider','Guided slider',(#17801));
#17851=PRODUCT('Slider housing','Slider housing','Slider housing',(#17801));
#17852=PRODUCT('Bushing cap','Bushing cap','Bushing cap',(#17801));
#17853=PRODUCT('Bushing cap (1)','Bushing cap (1)','Bushing cap (1)',(#17801));
#17854=PRODUCT('Slider pin','Slider pin','Slider pin',(#17801));
#17855=PRODUCT('Pin spacer 2 mm','Pin spacer 2 mm','Pin spacer 2 mm',(#17801));
#17856=PRODUCT('Pin spacer 4 mm (1)','Pin spacer 4 mm (1)',
'Pin spacer 4 mm (1)',(#17801));
#17857=PRODUCT('Pin keeper (1)','Pin keeper (1)','Pin keeper (1)',(#17801));
#17858=PRODUCT('Linear Ball Bushing - 12 x 21 x 30 mm',
'Linear Ball Bushing - 12 x 21 x 30 mm',
'Linear Ball Bushing - 12 x 21 x 30 mm',(#17801));
#17859=PRODUCT('Steel sleeve','Steel sleeve','Steel sleeve',(#17801));
#17860=PRODUCT('Ball retainer (plastic)','Ball retainer (plastic)',
'Ball retainer (plastic)',(#17801));
#17861=PRODUCT('M4x10 Cap Screw','M4x10 Cap Screw','M4x10 Cap Screw',(#17801));
#17862=PRESENTATION_STYLE_ASSIGNMENT((#17868));
#17863=PRESENTATION_STYLE_ASSIGNMENT((#17869));
#17864=PRESENTATION_STYLE_ASSIGNMENT((#17870));
#17865=PRESENTATION_STYLE_ASSIGNMENT((#17871));
#17866=PRESENTATION_STYLE_ASSIGNMENT((#17872));
#17867=PRESENTATION_STYLE_ASSIGNMENT((#17873));
#17868=SURFACE_STYLE_USAGE(.BOTH.,#17874);
#17869=SURFACE_STYLE_USAGE(.BOTH.,#17875);
#17870=SURFACE_STYLE_USAGE(.BOTH.,#17876);
#17871=SURFACE_STYLE_USAGE(.BOTH.,#17877);
#17872=SURFACE_STYLE_USAGE(.BOTH.,#17878);
#17873=SURFACE_STYLE_USAGE(.BOTH.,#17879);
#17874=SURFACE_SIDE_STYLE('',(#17880));
#17875=SURFACE_SIDE_STYLE('',(#17881));
#17876=SURFACE_SIDE_STYLE('',(#17882));
#17877=SURFACE_SIDE_STYLE('',(#17883));
#17878=SURFACE_SIDE_STYLE('',(#17884));
#17879=SURFACE_SIDE_STYLE('',(#17885));
#17880=SURFACE_STYLE_FILL_AREA(#17886);
#17881=SURFACE_STYLE_FILL_AREA(#17887);
#17882=SURFACE_STYLE_FILL_AREA(#17888);
#17883=SURFACE_STYLE_FILL_AREA(#17889);
#17884=SURFACE_STYLE_FILL_AREA(#17890);
#17885=SURFACE_STYLE_FILL_AREA(#17891);
#17886=FILL_AREA_STYLE('Steel - Satin',(#17892));
#17887=FILL_AREA_STYLE('CAD Library Painted - Deep blue',(#17893));
#17888=FILL_AREA_STYLE('CAD Library Painted - Steel gray',(#17894));
#17889=FILL_AREA_STYLE('CAD Library Painted - Graphite',(#17895));
#17890=FILL_AREA_STYLE('CAD Library Painted - Engineering blue',(#17896));
#17891=FILL_AREA_STYLE('CAD Library Painted - Light blue',(#17897));
#17892=FILL_AREA_STYLE_COLOUR('Steel - Satin',#17898);
#17893=FILL_AREA_STYLE_COLOUR('CAD Library Painted - Deep blue',#17899);
#17894=FILL_AREA_STYLE_COLOUR('CAD Library Painted - Steel gray',#17900);
#17895=FILL_AREA_STYLE_COLOUR('CAD Library Painted - Graphite',#17901);
#17896=FILL_AREA_STYLE_COLOUR('CAD Library Painted - Engineering blue',
#17902);
#17897=FILL_AREA_STYLE_COLOUR('CAD Library Painted - Light blue',#17903);
#17898=COLOUR_RGB('Steel - Satin',0.627450980392157,0.627450980392157,0.627450980392157);
#17899=COLOUR_RGB('CAD Library Painted - Deep blue',0.0784313725490196,
0.203921568627451,0.349019607843137);
#17900=COLOUR_RGB('CAD Library Painted - Steel gray',0.592156862745098,
0.631372549019608,0.67843137254902);
#17901=COLOUR_RGB('CAD Library Painted - Graphite',0.168627450980392,0.192156862745098,
0.231372549019608);
#17902=COLOUR_RGB('CAD Library Painted - Engineering blue',0.12156862745098,
0.356862745098039,0.6);
#17903=COLOUR_RGB('CAD Library Painted - Light blue',0.286274509803922,
0.552941176470588,0.780392156862745);
#17904=COLOUR_RGB('Dark Blue',0.08,0.2,0.34);
#17905=FILL_AREA_STYLE_COLOUR('',#17904);
#17906=FILL_AREA_STYLE('',(#17905));
#17907=SURFACE_STYLE_FILL_AREA(#17906);
#17908=SURFACE_SIDE_STYLE('',(#17907));
#17909=SURFACE_STYLE_USAGE(.BOTH.,#17908);
#17910=PRESENTATION_STYLE_ASSIGNMENT((#17909));
#17911=COLOUR_RGB('Light Blue',0.38,0.62,0.78);
#17912=FILL_AREA_STYLE_COLOUR('',#17911);
#17913=FILL_AREA_STYLE('',(#17912));
#17914=SURFACE_STYLE_FILL_AREA(#17913);
#17915=SURFACE_SIDE_STYLE('',(#17914));
#17916=SURFACE_STYLE_USAGE(.BOTH.,#17915);
#17917=PRESENTATION_STYLE_ASSIGNMENT((#17916));
#17918=COLOUR_RGB('Sky Blue',0.24,0.69,0.87);
#17919=FILL_AREA_STYLE_COLOUR('',#17918);
#17920=FILL_AREA_STYLE('',(#17919));
#17921=SURFACE_STYLE_FILL_AREA(#17920);
#17922=SURFACE_SIDE_STYLE('',(#17921));
#17923=SURFACE_STYLE_USAGE(.BOTH.,#17922);
#17924=PRESENTATION_STYLE_ASSIGNMENT((#17923));
#17925=COLOUR_RGB('Grey',0.48,0.52,0.57);
#17926=FILL_AREA_STYLE_COLOUR('',#17925);
#17927=FILL_AREA_STYLE('',(#17926));
#17928=SURFACE_STYLE_FILL_AREA(#17927);
#17929=SURFACE_SIDE_STYLE('',(#17928));
#17930=SURFACE_STYLE_USAGE(.BOTH.,#17929);
#17931=PRESENTATION_STYLE_ASSIGNMENT((#17930));
#17932=COLOUR_RGB('Black',0.12,0.14,0.17);
#17933=FILL_AREA_STYLE_COLOUR('',#17932);
#17934=FILL_AREA_STYLE('',(#17933));
#17935=SURFACE_STYLE_FILL_AREA(#17934);
#17936=SURFACE_SIDE_STYLE('',(#17935));
#17937=SURFACE_STYLE_USAGE(.BOTH.,#17936);
#17938=PRESENTATION_STYLE_ASSIGNMENT((#17937));
#17939=COLOUR_RGB('Off White',0.89,0.88,0.83);
#17940=FILL_AREA_STYLE_COLOUR('',#17939);
#17941=FILL_AREA_STYLE('',(#17940));
#17942=SURFACE_STYLE_FILL_AREA(#17941);
#17943=SURFACE_SIDE_STYLE('',(#17942));
#17944=SURFACE_STYLE_USAGE(.BOTH.,#17943);
#17945=PRESENTATION_STYLE_ASSIGNMENT((#17944));
ENDSEC;
END-ISO-10303-21;
